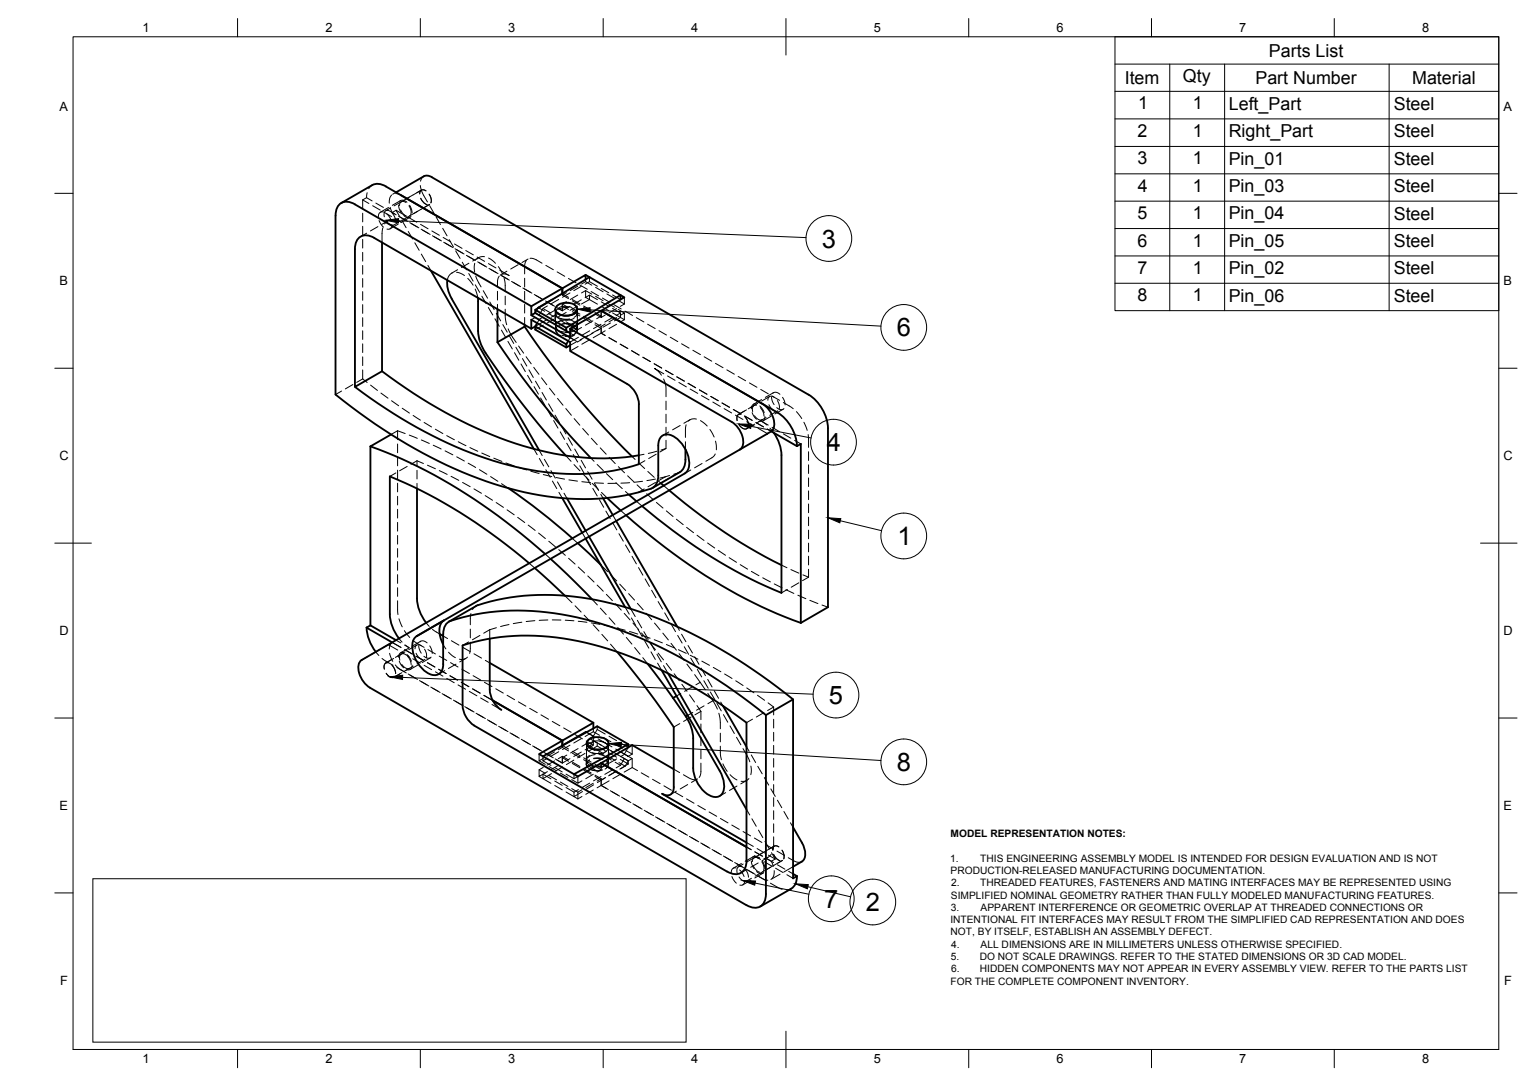
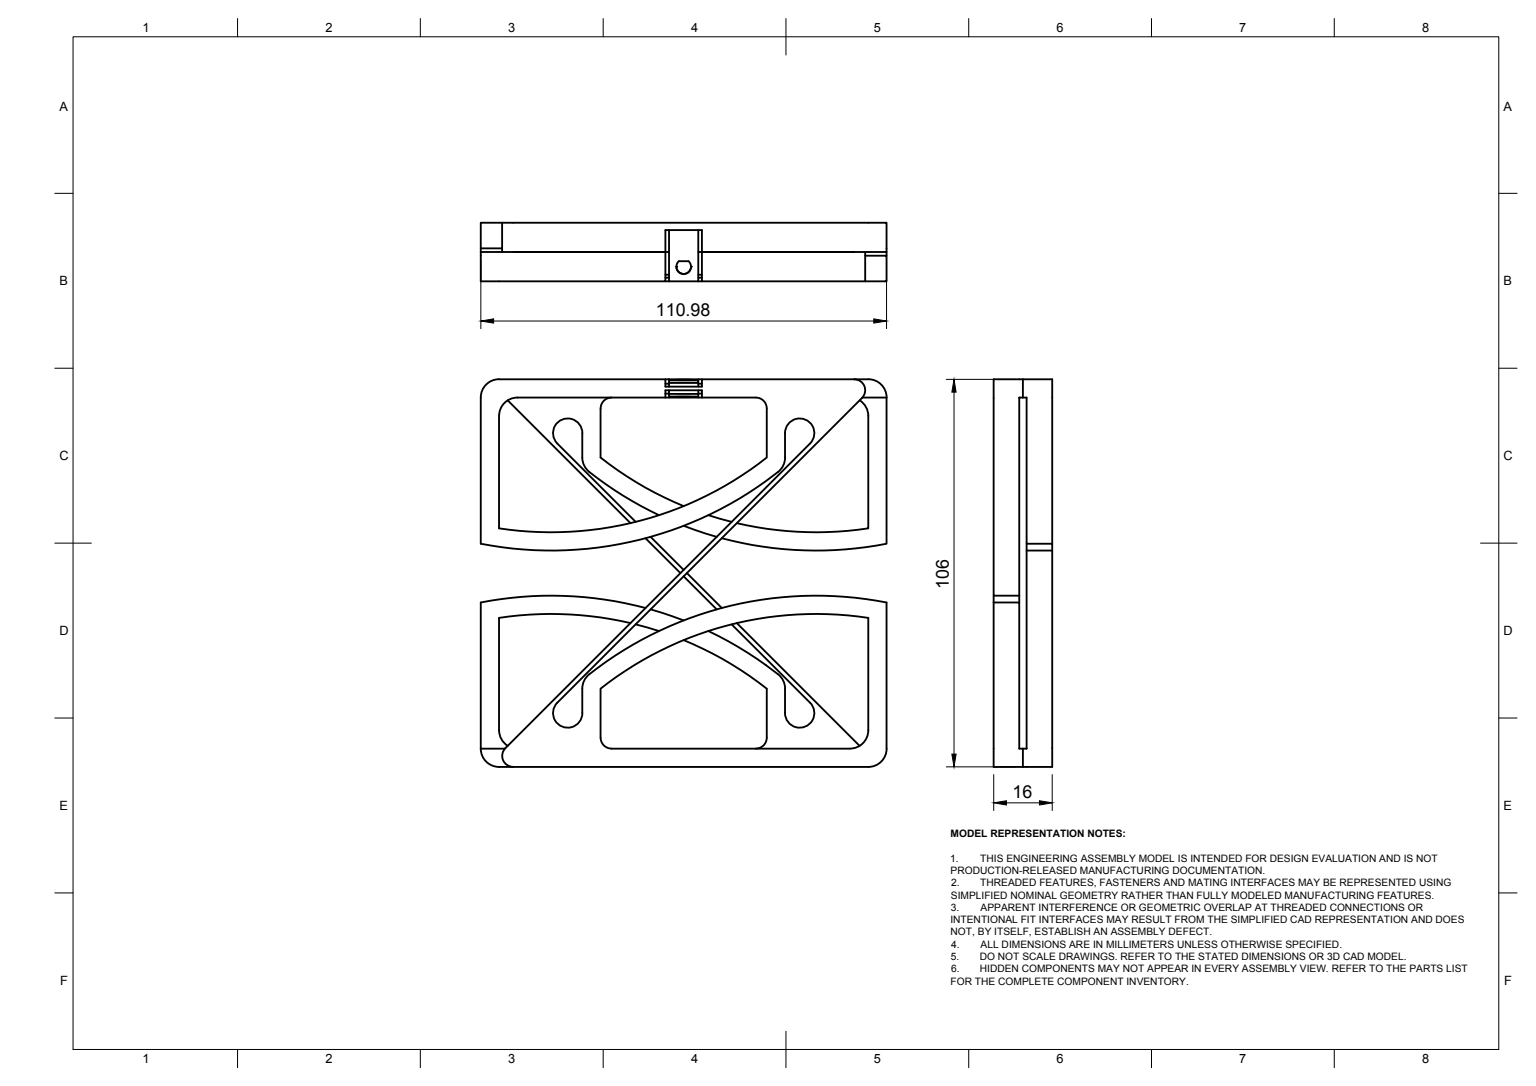
ISO-10303-21;
HEADER;
/* Generated by software containing ST-Developer
 * from STEP Tools, Inc. (www.steptools.com) 
 */

FILE_DESCRIPTION(
/* description */ (''),
/* implementation_level */ '2;1');

FILE_NAME(
/* name */ 'BR-159',
/* time_stamp */ '2026-10-05T13:12:53-07:00',
/* author */ (''),
/* organization */ (''),
/* preprocessor_version */ 'ST-DEVELOPER v20.2',
/* originating_system */ 'Autodesk Translation Framework v15.15.0.0',
/* authorisation */ '');

FILE_SCHEMA (('AUTOMOTIVE_DESIGN { 1 0 10303 214 3 1 1 }'));
ENDSEC;

DATA;
#10=MECHANICAL_DESIGN_GEOMETRIC_PRESENTATION_REPRESENTATION('',(#59,#60,
#61,#62,#63,#64,#65,#66),#5912);
#11=ITEM_DEFINED_TRANSFORMATION($,$,#3568,#3878);
#12=ITEM_DEFINED_TRANSFORMATION($,$,#3704,#3879);
#13=ITEM_DEFINED_TRANSFORMATION($,$,#3842,#3880);
#14=ITEM_DEFINED_TRANSFORMATION($,$,#3848,#3881);
#15=ITEM_DEFINED_TRANSFORMATION($,$,#3854,#3882);
#16=ITEM_DEFINED_TRANSFORMATION($,$,#3860,#3883);
#17=ITEM_DEFINED_TRANSFORMATION($,$,#3866,#3884);
#18=ITEM_DEFINED_TRANSFORMATION($,$,#3872,#3885);
#19=(
REPRESENTATION_RELATIONSHIP($,$,#5944,#5943)
REPRESENTATION_RELATIONSHIP_WITH_TRANSFORMATION(#11)
SHAPE_REPRESENTATION_RELATIONSHIP()
);
#20=(
REPRESENTATION_RELATIONSHIP($,$,#5945,#5943)
REPRESENTATION_RELATIONSHIP_WITH_TRANSFORMATION(#12)
SHAPE_REPRESENTATION_RELATIONSHIP()
);
#21=(
REPRESENTATION_RELATIONSHIP($,$,#5946,#5943)
REPRESENTATION_RELATIONSHIP_WITH_TRANSFORMATION(#13)
SHAPE_REPRESENTATION_RELATIONSHIP()
);
#22=(
REPRESENTATION_RELATIONSHIP($,$,#5947,#5943)
REPRESENTATION_RELATIONSHIP_WITH_TRANSFORMATION(#14)
SHAPE_REPRESENTATION_RELATIONSHIP()
);
#23=(
REPRESENTATION_RELATIONSHIP($,$,#5948,#5943)
REPRESENTATION_RELATIONSHIP_WITH_TRANSFORMATION(#15)
SHAPE_REPRESENTATION_RELATIONSHIP()
);
#24=(
REPRESENTATION_RELATIONSHIP($,$,#5949,#5943)
REPRESENTATION_RELATIONSHIP_WITH_TRANSFORMATION(#16)
SHAPE_REPRESENTATION_RELATIONSHIP()
);
#25=(
REPRESENTATION_RELATIONSHIP($,$,#5950,#5943)
REPRESENTATION_RELATIONSHIP_WITH_TRANSFORMATION(#17)
SHAPE_REPRESENTATION_RELATIONSHIP()
);
#26=(
REPRESENTATION_RELATIONSHIP($,$,#5951,#5943)
REPRESENTATION_RELATIONSHIP_WITH_TRANSFORMATION(#18)
SHAPE_REPRESENTATION_RELATIONSHIP()
);
#27=CONTEXT_DEPENDENT_SHAPE_REPRESENTATION(#19,#5935);
#28=CONTEXT_DEPENDENT_SHAPE_REPRESENTATION(#20,#5936);
#29=CONTEXT_DEPENDENT_SHAPE_REPRESENTATION(#21,#5937);
#30=CONTEXT_DEPENDENT_SHAPE_REPRESENTATION(#22,#5938);
#31=CONTEXT_DEPENDENT_SHAPE_REPRESENTATION(#23,#5939);
#32=CONTEXT_DEPENDENT_SHAPE_REPRESENTATION(#24,#5940);
#33=CONTEXT_DEPENDENT_SHAPE_REPRESENTATION(#25,#5941);
#34=CONTEXT_DEPENDENT_SHAPE_REPRESENTATION(#26,#5942);
#35=NEXT_ASSEMBLY_USAGE_OCCURRENCE('Left_Part:1','Left_Part:1',
'Left_Part:1',#5953,#5954,'Left_Part:1');
#36=NEXT_ASSEMBLY_USAGE_OCCURRENCE('Right_Part:1','Right_Part:1',
'Right_Part:1',#5953,#5955,'Right_Part:1');
#37=NEXT_ASSEMBLY_USAGE_OCCURRENCE('Pin_01:1','Pin_01:1','Pin_01:1',#5953,
#5956,'Pin_01:1');
#38=NEXT_ASSEMBLY_USAGE_OCCURRENCE('Pin_03:1','Pin_03:1','Pin_03:1',#5953,
#5957,'Pin_03:1');
#39=NEXT_ASSEMBLY_USAGE_OCCURRENCE('Pin_04:1','Pin_04:1','Pin_04:1',#5953,
#5958,'Pin_04:1');
#40=NEXT_ASSEMBLY_USAGE_OCCURRENCE('Pin_05:1','Pin_05:1','Pin_05:1',#5953,
#5959,'Pin_05:1');
#41=NEXT_ASSEMBLY_USAGE_OCCURRENCE('Pin_02:1','Pin_02:1','Pin_02:1',#5953,
#5960,'Pin_02:1');
#42=NEXT_ASSEMBLY_USAGE_OCCURRENCE('Pin_06:1','Pin_06:1','Pin_06:1',#5953,
#5961,'Pin_06:1');
#43=SHAPE_REPRESENTATION_RELATIONSHIP('SRR','None',#5944,#51);
#44=SHAPE_REPRESENTATION_RELATIONSHIP('SRR','None',#5945,#52);
#45=SHAPE_REPRESENTATION_RELATIONSHIP('SRR','None',#5946,#53);
#46=SHAPE_REPRESENTATION_RELATIONSHIP('SRR','None',#5947,#54);
#47=SHAPE_REPRESENTATION_RELATIONSHIP('SRR','None',#5948,#55);
#48=SHAPE_REPRESENTATION_RELATIONSHIP('SRR','None',#5949,#56);
#49=SHAPE_REPRESENTATION_RELATIONSHIP('SRR','None',#5950,#57);
#50=SHAPE_REPRESENTATION_RELATIONSHIP('SRR','None',#5951,#58);
#51=ADVANCED_BREP_SHAPE_REPRESENTATION('',(#67),#5904);
#52=ADVANCED_BREP_SHAPE_REPRESENTATION('',(#68),#5905);
#53=ADVANCED_BREP_SHAPE_REPRESENTATION('',(#69),#5906);
#54=ADVANCED_BREP_SHAPE_REPRESENTATION('',(#70),#5907);
#55=ADVANCED_BREP_SHAPE_REPRESENTATION('',(#71),#5908);
#56=ADVANCED_BREP_SHAPE_REPRESENTATION('',(#72),#5909);
#57=ADVANCED_BREP_SHAPE_REPRESENTATION('',(#73),#5910);
#58=ADVANCED_BREP_SHAPE_REPRESENTATION('',(#74),#5911);
#59=STYLED_ITEM('',(#5993),#67);
#60=STYLED_ITEM('',(#5993),#68);
#61=STYLED_ITEM('',(#5994),#69);
#62=STYLED_ITEM('',(#5994),#70);
#63=STYLED_ITEM('',(#5994),#71);
#64=STYLED_ITEM('',(#5994),#72);
#65=STYLED_ITEM('',(#5994),#73);
#66=STYLED_ITEM('',(#5994),#74);
#67=MANIFOLD_SOLID_BREP('Body1',#3470);
#68=MANIFOLD_SOLID_BREP('Body1',#3471);
#69=MANIFOLD_SOLID_BREP('Body1',#3472);
#70=MANIFOLD_SOLID_BREP('Body1',#3473);
#71=MANIFOLD_SOLID_BREP('Body1',#3474);
#72=MANIFOLD_SOLID_BREP('Body1',#3475);
#73=MANIFOLD_SOLID_BREP('Body1',#3476);
#74=MANIFOLD_SOLID_BREP('Body1',#3477);
#75=FACE_BOUND('',#374,.T.);
#76=FACE_BOUND('',#375,.T.);
#77=FACE_BOUND('',#379,.T.);
#78=FACE_BOUND('',#419,.T.);
#79=FACE_BOUND('',#421,.T.);
#80=FACE_BOUND('',#427,.T.);
#81=FACE_BOUND('',#428,.T.);
#82=FACE_BOUND('',#432,.T.);
#83=FACE_BOUND('',#437,.T.);
#84=FACE_BOUND('',#441,.T.);
#85=FACE_BOUND('',#442,.T.);
#86=FACE_BOUND('',#473,.T.);
#87=FACE_BOUND('',#474,.T.);
#88=FACE_BOUND('',#485,.T.);
#89=FACE_BOUND('',#489,.T.);
#90=FACE_BOUND('',#510,.T.);
#91=FACE_BOUND('',#511,.T.);
#92=FACE_BOUND('',#513,.T.);
#93=FACE_BOUND('',#515,.T.);
#94=FACE_BOUND('',#516,.T.);
#95=FACE_BOUND('',#522,.T.);
#96=ELLIPSE('',#3572,2.00043399581457,2.);
#97=ELLIPSE('',#3573,2.00173692551084,2.);
#98=ELLIPSE('',#3574,2.00173692551084,2.);
#99=ELLIPSE('',#3577,2.00043399581457,2.);
#100=ELLIPSE('',#3579,2.00043399581457,2.);
#101=ELLIPSE('',#3580,2.77129645175522,2.);
#102=ELLIPSE('',#3581,2.00043399581457,2.);
#103=ELLIPSE('',#3582,2.00043399581457,2.);
#104=ELLIPSE('',#3708,2.00043399581457,2.);
#105=ELLIPSE('',#3709,2.88922534092348,2.);
#106=ELLIPSE('',#3710,2.00043399581457,2.);
#107=ELLIPSE('',#3711,2.00173692551084,2.);
#108=ELLIPSE('',#3712,2.00173692551084,2.);
#109=ELLIPSE('',#3715,2.00043399581457,2.);
#110=ELLIPSE('',#3716,2.77129645175522,2.);
#111=ELLIPSE('',#3717,2.00043399581457,2.);
#112=ELLIPSE('',#3721,2.00043399581457,2.);
#113=ELLIPSE('',#3722,2.00043399581457,2.);
#114=CYLINDRICAL_SURFACE('',#3571,2.);
#115=CYLINDRICAL_SURFACE('',#3575,2.);
#116=CYLINDRICAL_SURFACE('',#3578,2.);
#117=CYLINDRICAL_SURFACE('',#3584,1.50000013517123);
#118=CYLINDRICAL_SURFACE('',#3588,1.4999996247669);
#119=CYLINDRICAL_SURFACE('',#3597,1.74999969554324);
#120=CYLINDRICAL_SURFACE('',#3601,4.99999999999999);
#121=CYLINDRICAL_SURFACE('',#3604,5.);
#122=CYLINDRICAL_SURFACE('',#3614,100.231846914414);
#123=CYLINDRICAL_SURFACE('',#3621,3.00000000000007);
#124=CYLINDRICAL_SURFACE('',#3625,95.2318469144141);
#125=CYLINDRICAL_SURFACE('',#3629,5.00000220964233);
#126=CYLINDRICAL_SURFACE('',#3633,3.99998589024062);
#127=CYLINDRICAL_SURFACE('',#3637,2.99999999999999);
#128=CYLINDRICAL_SURFACE('',#3640,3.00000000000001);
#129=CYLINDRICAL_SURFACE('',#3645,3.99998589024062);
#130=CYLINDRICAL_SURFACE('',#3649,5.00000220964233);
#131=CYLINDRICAL_SURFACE('',#3653,3.00000000000008);
#132=CYLINDRICAL_SURFACE('',#3656,2.99999999999999);
#133=CYLINDRICAL_SURFACE('',#3663,100.231846914414);
#134=CYLINDRICAL_SURFACE('',#3667,5.);
#135=CYLINDRICAL_SURFACE('',#3671,5.);
#136=CYLINDRICAL_SURFACE('',#3677,1.75000228959638);
#137=CYLINDRICAL_SURFACE('',#3694,95.231846914414);
#138=CYLINDRICAL_SURFACE('',#3707,2.);
#139=CYLINDRICAL_SURFACE('',#3713,2.);
#140=CYLINDRICAL_SURFACE('',#3720,2.);
#141=CYLINDRICAL_SURFACE('',#3723,1.50000013517123);
#142=CYLINDRICAL_SURFACE('',#3727,1.4999996247669);
#143=CYLINDRICAL_SURFACE('',#3732,5.);
#144=CYLINDRICAL_SURFACE('',#3735,5.);
#145=CYLINDRICAL_SURFACE('',#3739,1.75000228959638);
#146=CYLINDRICAL_SURFACE('',#3747,3.00000000000001);
#147=CYLINDRICAL_SURFACE('',#3751,3.99998589024062);
#148=CYLINDRICAL_SURFACE('',#3755,5.00000220964233);
#149=CYLINDRICAL_SURFACE('',#3758,95.231846914414);
#150=CYLINDRICAL_SURFACE('',#3762,3.00000000000008);
#151=CYLINDRICAL_SURFACE('',#3766,2.99999999999999);
#152=CYLINDRICAL_SURFACE('',#3779,100.231846914414);
#153=CYLINDRICAL_SURFACE('',#3794,1.74999969554324);
#154=CYLINDRICAL_SURFACE('',#3798,4.99999999999999);
#155=CYLINDRICAL_SURFACE('',#3801,5.);
#156=CYLINDRICAL_SURFACE('',#3820,100.231846914414);
#157=CYLINDRICAL_SURFACE('',#3832,3.00000000000007);
#158=CYLINDRICAL_SURFACE('',#3834,95.2318469144141);
#159=CYLINDRICAL_SURFACE('',#3836,5.00000220964233);
#160=CYLINDRICAL_SURFACE('',#3838,3.99998589024062);
#161=CYLINDRICAL_SURFACE('',#3840,2.99999999999999);
#162=CYLINDRICAL_SURFACE('',#3845,1.50000013517123);
#163=CYLINDRICAL_SURFACE('',#3849,1.4999996247669);
#164=CYLINDRICAL_SURFACE('',#3855,1.50000013517123);
#165=CYLINDRICAL_SURFACE('',#3861,2.);
#166=CYLINDRICAL_SURFACE('',#3869,1.4999996247669);
#167=CYLINDRICAL_SURFACE('',#3873,2.);
#168=FACE_OUTER_BOUND('',#350,.T.);
#169=FACE_OUTER_BOUND('',#351,.T.);
#170=FACE_OUTER_BOUND('',#352,.T.);
#171=FACE_OUTER_BOUND('',#353,.T.);
#172=FACE_OUTER_BOUND('',#354,.T.);
#173=FACE_OUTER_BOUND('',#355,.T.);
#174=FACE_OUTER_BOUND('',#356,.T.);
#175=FACE_OUTER_BOUND('',#357,.T.);
#176=FACE_OUTER_BOUND('',#358,.T.);
#177=FACE_OUTER_BOUND('',#359,.T.);
#178=FACE_OUTER_BOUND('',#360,.T.);
#179=FACE_OUTER_BOUND('',#361,.T.);
#180=FACE_OUTER_BOUND('',#362,.T.);
#181=FACE_OUTER_BOUND('',#363,.T.);
#182=FACE_OUTER_BOUND('',#364,.T.);
#183=FACE_OUTER_BOUND('',#365,.T.);
#184=FACE_OUTER_BOUND('',#366,.T.);
#185=FACE_OUTER_BOUND('',#367,.T.);
#186=FACE_OUTER_BOUND('',#368,.T.);
#187=FACE_OUTER_BOUND('',#369,.T.);
#188=FACE_OUTER_BOUND('',#370,.T.);
#189=FACE_OUTER_BOUND('',#371,.T.);
#190=FACE_OUTER_BOUND('',#372,.T.);
#191=FACE_OUTER_BOUND('',#373,.T.);
#192=FACE_OUTER_BOUND('',#376,.T.);
#193=FACE_OUTER_BOUND('',#377,.T.);
#194=FACE_OUTER_BOUND('',#378,.T.);
#195=FACE_OUTER_BOUND('',#380,.T.);
#196=FACE_OUTER_BOUND('',#381,.T.);
#197=FACE_OUTER_BOUND('',#382,.T.);
#198=FACE_OUTER_BOUND('',#383,.T.);
#199=FACE_OUTER_BOUND('',#384,.T.);
#200=FACE_OUTER_BOUND('',#385,.T.);
#201=FACE_OUTER_BOUND('',#386,.T.);
#202=FACE_OUTER_BOUND('',#387,.T.);
#203=FACE_OUTER_BOUND('',#388,.T.);
#204=FACE_OUTER_BOUND('',#389,.T.);
#205=FACE_OUTER_BOUND('',#390,.T.);
#206=FACE_OUTER_BOUND('',#391,.T.);
#207=FACE_OUTER_BOUND('',#392,.T.);
#208=FACE_OUTER_BOUND('',#393,.T.);
#209=FACE_OUTER_BOUND('',#394,.T.);
#210=FACE_OUTER_BOUND('',#395,.T.);
#211=FACE_OUTER_BOUND('',#396,.T.);
#212=FACE_OUTER_BOUND('',#397,.T.);
#213=FACE_OUTER_BOUND('',#398,.T.);
#214=FACE_OUTER_BOUND('',#399,.T.);
#215=FACE_OUTER_BOUND('',#400,.T.);
#216=FACE_OUTER_BOUND('',#401,.T.);
#217=FACE_OUTER_BOUND('',#402,.T.);
#218=FACE_OUTER_BOUND('',#403,.T.);
#219=FACE_OUTER_BOUND('',#404,.T.);
#220=FACE_OUTER_BOUND('',#405,.T.);
#221=FACE_OUTER_BOUND('',#406,.T.);
#222=FACE_OUTER_BOUND('',#407,.T.);
#223=FACE_OUTER_BOUND('',#408,.T.);
#224=FACE_OUTER_BOUND('',#409,.T.);
#225=FACE_OUTER_BOUND('',#410,.T.);
#226=FACE_OUTER_BOUND('',#411,.T.);
#227=FACE_OUTER_BOUND('',#412,.T.);
#228=FACE_OUTER_BOUND('',#413,.T.);
#229=FACE_OUTER_BOUND('',#414,.T.);
#230=FACE_OUTER_BOUND('',#415,.T.);
#231=FACE_OUTER_BOUND('',#416,.T.);
#232=FACE_OUTER_BOUND('',#417,.T.);
#233=FACE_OUTER_BOUND('',#418,.T.);
#234=FACE_OUTER_BOUND('',#420,.T.);
#235=FACE_OUTER_BOUND('',#422,.T.);
#236=FACE_OUTER_BOUND('',#423,.T.);
#237=FACE_OUTER_BOUND('',#424,.T.);
#238=FACE_OUTER_BOUND('',#425,.T.);
#239=FACE_OUTER_BOUND('',#426,.T.);
#240=FACE_OUTER_BOUND('',#429,.T.);
#241=FACE_OUTER_BOUND('',#430,.T.);
#242=FACE_OUTER_BOUND('',#431,.T.);
#243=FACE_OUTER_BOUND('',#433,.T.);
#244=FACE_OUTER_BOUND('',#434,.T.);
#245=FACE_OUTER_BOUND('',#435,.T.);
#246=FACE_OUTER_BOUND('',#436,.T.);
#247=FACE_OUTER_BOUND('',#438,.T.);
#248=FACE_OUTER_BOUND('',#439,.T.);
#249=FACE_OUTER_BOUND('',#440,.T.);
#250=FACE_OUTER_BOUND('',#443,.T.);
#251=FACE_OUTER_BOUND('',#444,.T.);
#252=FACE_OUTER_BOUND('',#445,.T.);
#253=FACE_OUTER_BOUND('',#446,.T.);
#254=FACE_OUTER_BOUND('',#447,.T.);
#255=FACE_OUTER_BOUND('',#448,.T.);
#256=FACE_OUTER_BOUND('',#449,.T.);
#257=FACE_OUTER_BOUND('',#450,.T.);
#258=FACE_OUTER_BOUND('',#451,.T.);
#259=FACE_OUTER_BOUND('',#452,.T.);
#260=FACE_OUTER_BOUND('',#453,.T.);
#261=FACE_OUTER_BOUND('',#454,.T.);
#262=FACE_OUTER_BOUND('',#455,.T.);
#263=FACE_OUTER_BOUND('',#456,.T.);
#264=FACE_OUTER_BOUND('',#457,.T.);
#265=FACE_OUTER_BOUND('',#458,.T.);
#266=FACE_OUTER_BOUND('',#459,.T.);
#267=FACE_OUTER_BOUND('',#460,.T.);
#268=FACE_OUTER_BOUND('',#461,.T.);
#269=FACE_OUTER_BOUND('',#462,.T.);
#270=FACE_OUTER_BOUND('',#463,.T.);
#271=FACE_OUTER_BOUND('',#464,.T.);
#272=FACE_OUTER_BOUND('',#465,.T.);
#273=FACE_OUTER_BOUND('',#466,.T.);
#274=FACE_OUTER_BOUND('',#467,.T.);
#275=FACE_OUTER_BOUND('',#468,.T.);
#276=FACE_OUTER_BOUND('',#469,.T.);
#277=FACE_OUTER_BOUND('',#470,.T.);
#278=FACE_OUTER_BOUND('',#471,.T.);
#279=FACE_OUTER_BOUND('',#472,.T.);
#280=FACE_OUTER_BOUND('',#475,.T.);
#281=FACE_OUTER_BOUND('',#476,.T.);
#282=FACE_OUTER_BOUND('',#477,.T.);
#283=FACE_OUTER_BOUND('',#478,.T.);
#284=FACE_OUTER_BOUND('',#479,.T.);
#285=FACE_OUTER_BOUND('',#480,.T.);
#286=FACE_OUTER_BOUND('',#481,.T.);
#287=FACE_OUTER_BOUND('',#482,.T.);
#288=FACE_OUTER_BOUND('',#483,.T.);
#289=FACE_OUTER_BOUND('',#484,.T.);
#290=FACE_OUTER_BOUND('',#486,.T.);
#291=FACE_OUTER_BOUND('',#487,.T.);
#292=FACE_OUTER_BOUND('',#488,.T.);
#293=FACE_OUTER_BOUND('',#490,.T.);
#294=FACE_OUTER_BOUND('',#491,.T.);
#295=FACE_OUTER_BOUND('',#492,.T.);
#296=FACE_OUTER_BOUND('',#493,.T.);
#297=FACE_OUTER_BOUND('',#494,.T.);
#298=FACE_OUTER_BOUND('',#495,.T.);
#299=FACE_OUTER_BOUND('',#496,.T.);
#300=FACE_OUTER_BOUND('',#497,.T.);
#301=FACE_OUTER_BOUND('',#498,.T.);
#302=FACE_OUTER_BOUND('',#499,.T.);
#303=FACE_OUTER_BOUND('',#500,.T.);
#304=FACE_OUTER_BOUND('',#501,.T.);
#305=FACE_OUTER_BOUND('',#502,.T.);
#306=FACE_OUTER_BOUND('',#503,.T.);
#307=FACE_OUTER_BOUND('',#504,.T.);
#308=FACE_OUTER_BOUND('',#505,.T.);
#309=FACE_OUTER_BOUND('',#506,.T.);
#310=FACE_OUTER_BOUND('',#507,.T.);
#311=FACE_OUTER_BOUND('',#508,.T.);
#312=FACE_OUTER_BOUND('',#509,.T.);
#313=FACE_OUTER_BOUND('',#512,.T.);
#314=FACE_OUTER_BOUND('',#514,.T.);
#315=FACE_OUTER_BOUND('',#517,.T.);
#316=FACE_OUTER_BOUND('',#518,.T.);
#317=FACE_OUTER_BOUND('',#519,.T.);
#318=FACE_OUTER_BOUND('',#520,.T.);
#319=FACE_OUTER_BOUND('',#521,.T.);
#320=FACE_OUTER_BOUND('',#523,.T.);
#321=FACE_OUTER_BOUND('',#524,.T.);
#322=FACE_OUTER_BOUND('',#525,.T.);
#323=FACE_OUTER_BOUND('',#526,.T.);
#324=FACE_OUTER_BOUND('',#527,.T.);
#325=FACE_OUTER_BOUND('',#528,.T.);
#326=FACE_OUTER_BOUND('',#529,.T.);
#327=FACE_OUTER_BOUND('',#530,.T.);
#328=FACE_OUTER_BOUND('',#531,.T.);
#329=FACE_OUTER_BOUND('',#532,.T.);
#330=FACE_OUTER_BOUND('',#533,.T.);
#331=FACE_OUTER_BOUND('',#534,.T.);
#332=FACE_OUTER_BOUND('',#535,.T.);
#333=FACE_OUTER_BOUND('',#536,.T.);
#334=FACE_OUTER_BOUND('',#537,.T.);
#335=FACE_OUTER_BOUND('',#538,.T.);
#336=FACE_OUTER_BOUND('',#539,.T.);
#337=FACE_OUTER_BOUND('',#540,.T.);
#338=FACE_OUTER_BOUND('',#541,.T.);
#339=FACE_OUTER_BOUND('',#542,.T.);
#340=FACE_OUTER_BOUND('',#543,.T.);
#341=FACE_OUTER_BOUND('',#544,.T.);
#342=FACE_OUTER_BOUND('',#545,.T.);
#343=FACE_OUTER_BOUND('',#546,.T.);
#344=FACE_OUTER_BOUND('',#547,.T.);
#345=FACE_OUTER_BOUND('',#548,.T.);
#346=FACE_OUTER_BOUND('',#549,.T.);
#347=FACE_OUTER_BOUND('',#550,.T.);
#348=FACE_OUTER_BOUND('',#551,.T.);
#349=FACE_OUTER_BOUND('',#552,.T.);
#350=EDGE_LOOP('',(#2190,#2191));
#351=EDGE_LOOP('',(#2192,#2193,#2194,#2195,#2196,#2197));
#352=EDGE_LOOP('',(#2198,#2199,#2200,#2201));
#353=EDGE_LOOP('',(#2202,#2203,#2204,#2205,#2206,#2207));
#354=EDGE_LOOP('',(#2208,#2209,#2210,#2211,#2212,#2213,#2214));
#355=EDGE_LOOP('',(#2215,#2216,#2217,#2218));
#356=EDGE_LOOP('',(#2219));
#357=EDGE_LOOP('',(#2220,#2221,#2222,#2223));
#358=EDGE_LOOP('',(#2224));
#359=EDGE_LOOP('',(#2225,#2226,#2227,#2228,#2229,#2230));
#360=EDGE_LOOP('',(#2231,#2232,#2233,#2234,#2235,#2236));
#361=EDGE_LOOP('',(#2237,#2238,#2239,#2240,#2241));
#362=EDGE_LOOP('',(#2242));
#363=EDGE_LOOP('',(#2243,#2244,#2245,#2246));
#364=EDGE_LOOP('',(#2247,#2248,#2249,#2250,#2251,#2252));
#365=EDGE_LOOP('',(#2253,#2254,#2255,#2256));
#366=EDGE_LOOP('',(#2257,#2258,#2259,#2260));
#367=EDGE_LOOP('',(#2261,#2262,#2263,#2264,#2265,#2266));
#368=EDGE_LOOP('',(#2267,#2268,#2269,#2270));
#369=EDGE_LOOP('',(#2271,#2272,#2273,#2274));
#370=EDGE_LOOP('',(#2275,#2276,#2277,#2278));
#371=EDGE_LOOP('',(#2279,#2280,#2281,#2282,#2283,#2284));
#372=EDGE_LOOP('',(#2285,#2286,#2287,#2288));
#373=EDGE_LOOP('',(#2289,#2290,#2291,#2292,#2293,#2294,#2295,#2296,#2297,
#2298,#2299,#2300));
#374=EDGE_LOOP('',(#2301));
#375=EDGE_LOOP('',(#2302));
#376=EDGE_LOOP('',(#2303,#2304,#2305,#2306));
#377=EDGE_LOOP('',(#2307,#2308,#2309,#2310,#2311,#2312));
#378=EDGE_LOOP('',(#2313,#2314,#2315,#2316));
#379=EDGE_LOOP('',(#2317));
#380=EDGE_LOOP('',(#2318,#2319,#2320,#2321,#2322,#2323));
#381=EDGE_LOOP('',(#2324,#2325,#2326,#2327,#2328,#2329));
#382=EDGE_LOOP('',(#2330,#2331,#2332,#2333));
#383=EDGE_LOOP('',(#2334,#2335,#2336,#2337));
#384=EDGE_LOOP('',(#2338,#2339,#2340,#2341));
#385=EDGE_LOOP('',(#2342,#2343,#2344,#2345));
#386=EDGE_LOOP('',(#2346,#2347,#2348,#2349));
#387=EDGE_LOOP('',(#2350,#2351,#2352,#2353));
#388=EDGE_LOOP('',(#2354,#2355,#2356,#2357));
#389=EDGE_LOOP('',(#2358,#2359,#2360,#2361,#2362));
#390=EDGE_LOOP('',(#2363,#2364,#2365,#2366,#2367,#2368,#2369));
#391=EDGE_LOOP('',(#2370,#2371,#2372,#2373,#2374));
#392=EDGE_LOOP('',(#2375,#2376,#2377,#2378));
#393=EDGE_LOOP('',(#2379,#2380,#2381,#2382));
#394=EDGE_LOOP('',(#2383,#2384,#2385,#2386));
#395=EDGE_LOOP('',(#2387,#2388,#2389,#2390));
#396=EDGE_LOOP('',(#2391,#2392,#2393,#2394));
#397=EDGE_LOOP('',(#2395,#2396,#2397,#2398));
#398=EDGE_LOOP('',(#2399,#2400,#2401,#2402));
#399=EDGE_LOOP('',(#2403,#2404,#2405,#2406));
#400=EDGE_LOOP('',(#2407,#2408,#2409,#2410));
#401=EDGE_LOOP('',(#2411,#2412,#2413,#2414,#2415,#2416));
#402=EDGE_LOOP('',(#2417,#2418,#2419,#2420,#2421,#2422));
#403=EDGE_LOOP('',(#2423,#2424,#2425,#2426));
#404=EDGE_LOOP('',(#2427,#2428,#2429,#2430));
#405=EDGE_LOOP('',(#2431,#2432,#2433,#2434));
#406=EDGE_LOOP('',(#2435,#2436,#2437,#2438,#2439));
#407=EDGE_LOOP('',(#2440,#2441,#2442,#2443,#2444,#2445,#2446,#2447,#2448,
#2449,#2450));
#408=EDGE_LOOP('',(#2451,#2452,#2453,#2454));
#409=EDGE_LOOP('',(#2455,#2456,#2457,#2458));
#410=EDGE_LOOP('',(#2459,#2460,#2461,#2462,#2463,#2464,#2465,#2466,#2467,
#2468,#2469,#2470,#2471,#2472,#2473,#2474,#2475,#2476,#2477,#2478,#2479,
#2480,#2481,#2482,#2483,#2484,#2485,#2486,#2487));
#411=EDGE_LOOP('',(#2488,#2489,#2490,#2491));
#412=EDGE_LOOP('',(#2492));
#413=EDGE_LOOP('',(#2493,#2494,#2495,#2496));
#414=EDGE_LOOP('',(#2497,#2498,#2499,#2500,#2501,#2502,#2503,#2504));
#415=EDGE_LOOP('',(#2505,#2506,#2507,#2508));
#416=EDGE_LOOP('',(#2509,#2510,#2511,#2512));
#417=EDGE_LOOP('',(#2513,#2514,#2515,#2516));
#418=EDGE_LOOP('',(#2517,#2518,#2519,#2520));
#419=EDGE_LOOP('',(#2521));
#420=EDGE_LOOP('',(#2522,#2523,#2524,#2525));
#421=EDGE_LOOP('',(#2526));
#422=EDGE_LOOP('',(#2527,#2528,#2529,#2530));
#423=EDGE_LOOP('',(#2531,#2532,#2533,#2534));
#424=EDGE_LOOP('',(#2535,#2536,#2537,#2538,#2539,#2540));
#425=EDGE_LOOP('',(#2541,#2542,#2543,#2544,#2545,#2546));
#426=EDGE_LOOP('',(#2547,#2548,#2549,#2550,#2551,#2552,#2553,#2554,#2555,
#2556,#2557,#2558,#2559,#2560,#2561,#2562,#2563,#2564,#2565,#2566,#2567,
#2568,#2569));
#427=EDGE_LOOP('',(#2570,#2571,#2572,#2573,#2574,#2575,#2576,#2577,#2578,
#2579));
#428=EDGE_LOOP('',(#2580,#2581,#2582,#2583,#2584,#2585));
#429=EDGE_LOOP('',(#2586,#2587,#2588,#2589));
#430=EDGE_LOOP('',(#2590,#2591,#2592,#2593,#2594,#2595,#2596,#2597,#2598,
#2599,#2600,#2601,#2602,#2603));
#431=EDGE_LOOP('',(#2604,#2605,#2606,#2607));
#432=EDGE_LOOP('',(#2608,#2609,#2610));
#433=EDGE_LOOP('',(#2611,#2612,#2613,#2614));
#434=EDGE_LOOP('',(#2615,#2616,#2617,#2618));
#435=EDGE_LOOP('',(#2619,#2620,#2621,#2622));
#436=EDGE_LOOP('',(#2623,#2624,#2625,#2626));
#437=EDGE_LOOP('',(#2627));
#438=EDGE_LOOP('',(#2628,#2629,#2630,#2631,#2632,#2633,#2634,#2635));
#439=EDGE_LOOP('',(#2636,#2637,#2638,#2639));
#440=EDGE_LOOP('',(#2640,#2641,#2642,#2643,#2644,#2645,#2646,#2647,#2648,
#2649,#2650,#2651));
#441=EDGE_LOOP('',(#2652));
#442=EDGE_LOOP('',(#2653));
#443=EDGE_LOOP('',(#2654,#2655));
#444=EDGE_LOOP('',(#2656,#2657,#2658,#2659,#2660,#2661,#2662,#2663));
#445=EDGE_LOOP('',(#2664,#2665,#2666,#2667,#2668,#2669));
#446=EDGE_LOOP('',(#2670,#2671,#2672,#2673,#2674,#2675,#2676));
#447=EDGE_LOOP('',(#2677,#2678,#2679,#2680,#2681,#2682,#2683));
#448=EDGE_LOOP('',(#2684,#2685,#2686,#2687));
#449=EDGE_LOOP('',(#2688,#2689,#2690,#2691));
#450=EDGE_LOOP('',(#2692));
#451=EDGE_LOOP('',(#2693,#2694,#2695,#2696));
#452=EDGE_LOOP('',(#2697));
#453=EDGE_LOOP('',(#2698,#2699,#2700,#2701));
#454=EDGE_LOOP('',(#2702,#2703,#2704,#2705,#2706));
#455=EDGE_LOOP('',(#2707,#2708,#2709,#2710));
#456=EDGE_LOOP('',(#2711,#2712,#2713,#2714));
#457=EDGE_LOOP('',(#2715,#2716,#2717,#2718));
#458=EDGE_LOOP('',(#2719));
#459=EDGE_LOOP('',(#2720,#2721,#2722,#2723));
#460=EDGE_LOOP('',(#2724,#2725,#2726,#2727));
#461=EDGE_LOOP('',(#2728,#2729,#2730,#2731,#2732,#2733));
#462=EDGE_LOOP('',(#2734,#2735,#2736,#2737,#2738,#2739));
#463=EDGE_LOOP('',(#2740,#2741,#2742,#2743,#2744));
#464=EDGE_LOOP('',(#2745,#2746,#2747,#2748));
#465=EDGE_LOOP('',(#2749,#2750,#2751,#2752));
#466=EDGE_LOOP('',(#2753,#2754,#2755,#2756));
#467=EDGE_LOOP('',(#2757,#2758,#2759,#2760));
#468=EDGE_LOOP('',(#2761,#2762,#2763,#2764));
#469=EDGE_LOOP('',(#2765,#2766,#2767,#2768));
#470=EDGE_LOOP('',(#2769,#2770,#2771,#2772,#2773,#2774,#2775,#2776,#2777,
#2778,#2779,#2780,#2781,#2782));
#471=EDGE_LOOP('',(#2783,#2784,#2785,#2786));
#472=EDGE_LOOP('',(#2787,#2788,#2789,#2790,#2791,#2792,#2793,#2794,#2795,
#2796,#2797,#2798));
#473=EDGE_LOOP('',(#2799));
#474=EDGE_LOOP('',(#2800));
#475=EDGE_LOOP('',(#2801,#2802,#2803,#2804));
#476=EDGE_LOOP('',(#2805,#2806,#2807,#2808));
#477=EDGE_LOOP('',(#2809,#2810,#2811,#2812));
#478=EDGE_LOOP('',(#2813,#2814,#2815,#2816,#2817,#2818));
#479=EDGE_LOOP('',(#2819,#2820,#2821,#2822,#2823,#2824,#2825,#2826));
#480=EDGE_LOOP('',(#2827,#2828,#2829,#2830,#2831,#2832));
#481=EDGE_LOOP('',(#2833,#2834,#2835,#2836));
#482=EDGE_LOOP('',(#2837,#2838,#2839,#2840));
#483=EDGE_LOOP('',(#2841,#2842,#2843,#2844,#2845,#2846));
#484=EDGE_LOOP('',(#2847,#2848,#2849,#2850));
#485=EDGE_LOOP('',(#2851));
#486=EDGE_LOOP('',(#2852,#2853,#2854,#2855));
#487=EDGE_LOOP('',(#2856,#2857,#2858,#2859,#2860,#2861,#2862,#2863,#2864,
#2865,#2866));
#488=EDGE_LOOP('',(#2867,#2868,#2869,#2870));
#489=EDGE_LOOP('',(#2871,#2872,#2873));
#490=EDGE_LOOP('',(#2874,#2875,#2876,#2877));
#491=EDGE_LOOP('',(#2878,#2879,#2880,#2881));
#492=EDGE_LOOP('',(#2882,#2883,#2884,#2885,#2886,#2887));
#493=EDGE_LOOP('',(#2888,#2889,#2890,#2891,#2892,#2893,#2894,#2895));
#494=EDGE_LOOP('',(#2896,#2897,#2898,#2899));
#495=EDGE_LOOP('',(#2900,#2901,#2902,#2903,#2904,#2905));
#496=EDGE_LOOP('',(#2906,#2907,#2908,#2909,#2910,#2911));
#497=EDGE_LOOP('',(#2912,#2913,#2914,#2915,#2916));
#498=EDGE_LOOP('',(#2917));
#499=EDGE_LOOP('',(#2918,#2919,#2920,#2921));
#500=EDGE_LOOP('',(#2922,#2923,#2924,#2925,#2926,#2927));
#501=EDGE_LOOP('',(#2928,#2929,#2930,#2931));
#502=EDGE_LOOP('',(#2932,#2933,#2934,#2935));
#503=EDGE_LOOP('',(#2936,#2937,#2938,#2939,#2940,#2941));
#504=EDGE_LOOP('',(#2942,#2943,#2944,#2945));
#505=EDGE_LOOP('',(#2946,#2947,#2948,#2949));
#506=EDGE_LOOP('',(#2950,#2951,#2952,#2953));
#507=EDGE_LOOP('',(#2954,#2955,#2956,#2957));
#508=EDGE_LOOP('',(#2958,#2959,#2960,#2961));
#509=EDGE_LOOP('',(#2962,#2963,#2964,#2965,#2966,#2967,#2968,#2969,#2970,
#2971,#2972,#2973,#2974,#2975,#2976,#2977,#2978,#2979,#2980,#2981,#2982,
#2983,#2984));
#510=EDGE_LOOP('',(#2985,#2986,#2987,#2988,#2989,#2990,#2991,#2992,#2993,
#2994));
#511=EDGE_LOOP('',(#2995,#2996,#2997,#2998,#2999,#3000));
#512=EDGE_LOOP('',(#3001,#3002,#3003,#3004));
#513=EDGE_LOOP('',(#3005));
#514=EDGE_LOOP('',(#3006,#3007,#3008,#3009,#3010,#3011,#3012,#3013,#3014,
#3015,#3016,#3017));
#515=EDGE_LOOP('',(#3018));
#516=EDGE_LOOP('',(#3019));
#517=EDGE_LOOP('',(#3020,#3021,#3022,#3023));
#518=EDGE_LOOP('',(#3024,#3025,#3026,#3027));
#519=EDGE_LOOP('',(#3028,#3029,#3030,#3031,#3032,#3033,#3034,#3035,#3036,
#3037,#3038,#3039,#3040,#3041,#3042,#3043,#3044,#3045,#3046,#3047,#3048,
#3049,#3050,#3051,#3052,#3053,#3054,#3055,#3056));
#520=EDGE_LOOP('',(#3057,#3058,#3059,#3060,#3061,#3062));
#521=EDGE_LOOP('',(#3063,#3064,#3065,#3066));
#522=EDGE_LOOP('',(#3067));
#523=EDGE_LOOP('',(#3068,#3069,#3070,#3071,#3072,#3073));
#524=EDGE_LOOP('',(#3074,#3075,#3076,#3077,#3078,#3079));
#525=EDGE_LOOP('',(#3080,#3081,#3082,#3083));
#526=EDGE_LOOP('',(#3084,#3085,#3086,#3087));
#527=EDGE_LOOP('',(#3088,#3089,#3090,#3091));
#528=EDGE_LOOP('',(#3092,#3093,#3094,#3095));
#529=EDGE_LOOP('',(#3096,#3097,#3098,#3099));
#530=EDGE_LOOP('',(#3100,#3101,#3102,#3103));
#531=EDGE_LOOP('',(#3104,#3105,#3106,#3107));
#532=EDGE_LOOP('',(#3108,#3109,#3110,#3111,#3112));
#533=EDGE_LOOP('',(#3113,#3114,#3115,#3116,#3117,#3118,#3119));
#534=EDGE_LOOP('',(#3120,#3121,#3122,#3123));
#535=EDGE_LOOP('',(#3124));
#536=EDGE_LOOP('',(#3125,#3126,#3127,#3128));
#537=EDGE_LOOP('',(#3129));
#538=EDGE_LOOP('',(#3130,#3131,#3132,#3133));
#539=EDGE_LOOP('',(#3134));
#540=EDGE_LOOP('',(#3135));
#541=EDGE_LOOP('',(#3136,#3137,#3138,#3139));
#542=EDGE_LOOP('',(#3140));
#543=EDGE_LOOP('',(#3141));
#544=EDGE_LOOP('',(#3142,#3143,#3144,#3145));
#545=EDGE_LOOP('',(#3146));
#546=EDGE_LOOP('',(#3147));
#547=EDGE_LOOP('',(#3148));
#548=EDGE_LOOP('',(#3149,#3150,#3151,#3152));
#549=EDGE_LOOP('',(#3153));
#550=EDGE_LOOP('',(#3154,#3155,#3156,#3157));
#551=EDGE_LOOP('',(#3158));
#552=EDGE_LOOP('',(#3159));
#553=CIRCLE('',#3570,2.);
#554=CIRCLE('',#3576,2.);
#555=CIRCLE('',#3585,1.50000013517123);
#556=CIRCLE('',#3586,1.50000013517123);
#557=CIRCLE('',#3589,1.4999996247669);
#558=CIRCLE('',#3590,1.4999996247669);
#559=CIRCLE('',#3596,1.74999969554324);
#560=CIRCLE('',#3598,1.74999969554324);
#561=CIRCLE('',#3602,4.99999999999999);
#562=CIRCLE('',#3603,4.99999999999999);
#563=CIRCLE('',#3605,5.);
#564=CIRCLE('',#3606,5.);
#565=CIRCLE('',#3613,2.99999999999999);
#566=CIRCLE('',#3615,100.231846914414);
#567=CIRCLE('',#3616,100.231846914414);
#568=CIRCLE('',#3622,3.00000000000007);
#569=CIRCLE('',#3623,3.00000000000007);
#570=CIRCLE('',#3626,95.2318469144141);
#571=CIRCLE('',#3627,95.2318469144141);
#572=CIRCLE('',#3630,5.00000220964233);
#573=CIRCLE('',#3631,5.00000220964233);
#574=CIRCLE('',#3634,3.99998589024062);
#575=CIRCLE('',#3635,3.99998589024062);
#576=CIRCLE('',#3638,2.99999999999999);
#577=CIRCLE('',#3639,2.99999999999999);
#578=CIRCLE('',#3641,3.00000000000001);
#579=CIRCLE('',#3642,3.00000000000001);
#580=CIRCLE('',#3643,3.00000000000001);
#581=CIRCLE('',#3646,3.99998589024062);
#582=CIRCLE('',#3647,3.99998589024062);
#583=CIRCLE('',#3650,5.00000220964233);
#584=CIRCLE('',#3651,5.00000220964233);
#585=CIRCLE('',#3654,3.00000000000008);
#586=CIRCLE('',#3655,3.00000000000008);
#587=CIRCLE('',#3657,2.99999999999999);
#588=CIRCLE('',#3664,100.231846914414);
#589=CIRCLE('',#3665,100.231846914414);
#590=CIRCLE('',#3668,5.);
#591=CIRCLE('',#3669,5.);
#592=CIRCLE('',#3672,5.);
#593=CIRCLE('',#3673,5.);
#594=CIRCLE('',#3676,95.231846914414);
#595=CIRCLE('',#3678,1.75000228959638);
#596=CIRCLE('',#3679,1.75000228959638);
#597=CIRCLE('',#3693,95.231846914414);
#598=CIRCLE('',#3706,2.);
#599=CIRCLE('',#3714,2.);
#600=CIRCLE('',#3724,1.50000013517123);
#601=CIRCLE('',#3725,1.50000013517123);
#602=CIRCLE('',#3728,1.4999996247669);
#603=CIRCLE('',#3729,1.4999996247669);
#604=CIRCLE('',#3733,5.);
#605=CIRCLE('',#3734,5.);
#606=CIRCLE('',#3736,5.);
#607=CIRCLE('',#3737,5.);
#608=CIRCLE('',#3740,1.75000228959638);
#609=CIRCLE('',#3741,1.75000228959638);
#610=CIRCLE('',#3748,3.00000000000001);
#611=CIRCLE('',#3749,3.00000000000001);
#612=CIRCLE('',#3750,3.00000000000001);
#613=CIRCLE('',#3752,3.99998589024062);
#614=CIRCLE('',#3753,3.99998589024062);
#615=CIRCLE('',#3756,5.00000220964233);
#616=CIRCLE('',#3757,5.00000220964233);
#617=CIRCLE('',#3759,95.231846914414);
#618=CIRCLE('',#3760,95.231846914414);
#619=CIRCLE('',#3763,3.00000000000008);
#620=CIRCLE('',#3764,3.00000000000008);
#621=CIRCLE('',#3767,2.99999999999999);
#622=CIRCLE('',#3780,100.231846914414);
#623=CIRCLE('',#3781,100.231846914414);
#624=CIRCLE('',#3793,1.74999969554324);
#625=CIRCLE('',#3795,1.74999969554324);
#626=CIRCLE('',#3799,4.99999999999999);
#627=CIRCLE('',#3800,4.99999999999999);
#628=CIRCLE('',#3802,5.);
#629=CIRCLE('',#3803,5.);
#630=CIRCLE('',#3810,2.99999999999999);
#631=CIRCLE('',#3811,100.231846914414);
#632=CIRCLE('',#3812,5.00000220964233);
#633=CIRCLE('',#3813,3.99998589024062);
#634=CIRCLE('',#3814,3.00000000000007);
#635=CIRCLE('',#3815,95.2318469144141);
#636=CIRCLE('',#3818,2.99999999999999);
#637=CIRCLE('',#3821,100.231846914414);
#638=CIRCLE('',#3823,3.99998589024062);
#639=CIRCLE('',#3824,5.00000220964233);
#640=CIRCLE('',#3825,95.2318469144141);
#641=CIRCLE('',#3826,3.00000000000007);
#642=CIRCLE('',#3827,2.99999999999999);
#643=CIRCLE('',#3844,1.50000013517123);
#644=CIRCLE('',#3846,1.50000013517123);
#645=CIRCLE('',#3850,1.4999996247669);
#646=CIRCLE('',#3851,1.4999996247669);
#647=CIRCLE('',#3856,1.50000013517123);
#648=CIRCLE('',#3857,1.50000013517123);
#649=CIRCLE('',#3862,2.);
#650=CIRCLE('',#3863,2.);
#651=CIRCLE('',#3868,1.4999996247669);
#652=CIRCLE('',#3870,1.4999996247669);
#653=CIRCLE('',#3874,2.);
#654=CIRCLE('',#3875,2.);
#655=LINE('',#4894,#1020);
#656=LINE('',#4900,#1021);
#657=LINE('',#4907,#1022);
#658=LINE('',#4917,#1023);
#659=LINE('',#4921,#1024);
#660=LINE('',#4923,#1025);
#661=LINE('',#4925,#1026);
#662=LINE('',#4927,#1027);
#663=LINE('',#4928,#1028);
#664=LINE('',#4933,#1029);
#665=LINE('',#4940,#1030);
#666=LINE('',#4945,#1031);
#667=LINE('',#4947,#1032);
#668=LINE('',#4949,#1033);
#669=LINE('',#4951,#1034);
#670=LINE('',#4952,#1035);
#671=LINE('',#4956,#1036);
#672=LINE('',#4958,#1037);
#673=LINE('',#4960,#1038);
#674=LINE('',#4962,#1039);
#675=LINE('',#4964,#1040);
#676=LINE('',#4965,#1041);
#677=LINE('',#4968,#1042);
#678=LINE('',#4970,#1043);
#679=LINE('',#4972,#1044);
#680=LINE('',#4973,#1045);
#681=LINE('',#4979,#1046);
#682=LINE('',#4983,#1047);
#683=LINE('',#4985,#1048);
#684=LINE('',#4987,#1049);
#685=LINE('',#4989,#1050);
#686=LINE('',#4990,#1051);
#687=LINE('',#4994,#1052);
#688=LINE('',#4996,#1053);
#689=LINE('',#4998,#1054);
#690=LINE('',#4999,#1055);
#691=LINE('',#5007,#1056);
#692=LINE('',#5010,#1057);
#693=LINE('',#5012,#1058);
#694=LINE('',#5013,#1059);
#695=LINE('',#5016,#1060);
#696=LINE('',#5018,#1061);
#697=LINE('',#5019,#1062);
#698=LINE('',#5022,#1063);
#699=LINE('',#5023,#1064);
#700=LINE('',#5026,#1065);
#701=LINE('',#5027,#1066);
#702=LINE('',#5030,#1067);
#703=LINE('',#5031,#1068);
#704=LINE('',#5034,#1069);
#705=LINE('',#5036,#1070);
#706=LINE('',#5038,#1071);
#707=LINE('',#5042,#1072);
#708=LINE('',#5043,#1073);
#709=LINE('',#5048,#1074);
#710=LINE('',#5052,#1075);
#711=LINE('',#5053,#1076);
#712=LINE('',#5055,#1077);
#713=LINE('',#5058,#1078);
#714=LINE('',#5059,#1079);
#715=LINE('',#5062,#1080);
#716=LINE('',#5064,#1081);
#717=LINE('',#5066,#1082);
#718=LINE('',#5067,#1083);
#719=LINE('',#5073,#1084);
#720=LINE('',#5076,#1085);
#721=LINE('',#5078,#1086);
#722=LINE('',#5079,#1087);
#723=LINE('',#5085,#1088);
#724=LINE('',#5087,#1089);
#725=LINE('',#5088,#1090);
#726=LINE('',#5094,#1091);
#727=LINE('',#5097,#1092);
#728=LINE('',#5099,#1093);
#729=LINE('',#5100,#1094);
#730=LINE('',#5106,#1095);
#731=LINE('',#5109,#1096);
#732=LINE('',#5111,#1097);
#733=LINE('',#5112,#1098);
#734=LINE('',#5117,#1099);
#735=LINE('',#5124,#1100);
#736=LINE('',#5129,#1101);
#737=LINE('',#5132,#1102);
#738=LINE('',#5134,#1103);
#739=LINE('',#5135,#1104);
#740=LINE('',#5140,#1105);
#741=LINE('',#5144,#1106);
#742=LINE('',#5146,#1107);
#743=LINE('',#5147,#1108);
#744=LINE('',#5152,#1109);
#745=LINE('',#5157,#1110);
#746=LINE('',#5159,#1111);
#747=LINE('',#5161,#1112);
#748=LINE('',#5162,#1113);
#749=LINE('',#5167,#1114);
#750=LINE('',#5171,#1115);
#751=LINE('',#5174,#1116);
#752=LINE('',#5178,#1117);
#753=LINE('',#5180,#1118);
#754=LINE('',#5182,#1119);
#755=LINE('',#5183,#1120);
#756=LINE('',#5187,#1121);
#757=LINE('',#5189,#1122);
#758=LINE('',#5191,#1123);
#759=LINE('',#5192,#1124);
#760=LINE('',#5196,#1125);
#761=LINE('',#5198,#1126);
#762=LINE('',#5200,#1127);
#763=LINE('',#5202,#1128);
#764=LINE('',#5204,#1129);
#765=LINE('',#5205,#1130);
#766=LINE('',#5209,#1131);
#767=LINE('',#5211,#1132);
#768=LINE('',#5213,#1133);
#769=LINE('',#5215,#1134);
#770=LINE('',#5217,#1135);
#771=LINE('',#5218,#1136);
#772=LINE('',#5220,#1137);
#773=LINE('',#5221,#1138);
#774=LINE('',#5226,#1139);
#775=LINE('',#5230,#1140);
#776=LINE('',#5232,#1141);
#777=LINE('',#5233,#1142);
#778=LINE('',#5238,#1143);
#779=LINE('',#5241,#1144);
#780=LINE('',#5244,#1145);
#781=LINE('',#5246,#1146);
#782=LINE('',#5248,#1147);
#783=LINE('',#5249,#1148);
#784=LINE('',#5250,#1149);
#785=LINE('',#5251,#1150);
#786=LINE('',#5252,#1151);
#787=LINE('',#5258,#1152);
#788=LINE('',#5261,#1153);
#789=LINE('',#5264,#1154);
#790=LINE('',#5266,#1155);
#791=LINE('',#5267,#1156);
#792=LINE('',#5269,#1157);
#793=LINE('',#5271,#1158);
#794=LINE('',#5276,#1159);
#795=LINE('',#5282,#1160);
#796=LINE('',#5284,#1161);
#797=LINE('',#5286,#1162);
#798=LINE('',#5287,#1163);
#799=LINE('',#5290,#1164);
#800=LINE('',#5291,#1165);
#801=LINE('',#5293,#1166);
#802=LINE('',#5294,#1167);
#803=LINE('',#5297,#1168);
#804=LINE('',#5298,#1169);
#805=LINE('',#5300,#1170);
#806=LINE('',#5303,#1171);
#807=LINE('',#5305,#1172);
#808=LINE('',#5306,#1173);
#809=LINE('',#5308,#1174);
#810=LINE('',#5311,#1175);
#811=LINE('',#5312,#1176);
#812=LINE('',#5315,#1177);
#813=LINE('',#5316,#1178);
#814=LINE('',#5318,#1179);
#815=LINE('',#5323,#1180);
#816=LINE('',#5325,#1181);
#817=LINE('',#5327,#1182);
#818=LINE('',#5329,#1183);
#819=LINE('',#5331,#1184);
#820=LINE('',#5332,#1185);
#821=LINE('',#5335,#1186);
#822=LINE('',#5338,#1187);
#823=LINE('',#5339,#1188);
#824=LINE('',#5340,#1189);
#825=LINE('',#5341,#1190);
#826=LINE('',#5342,#1191);
#827=LINE('',#5344,#1192);
#828=LINE('',#5346,#1193);
#829=LINE('',#5348,#1194);
#830=LINE('',#5350,#1195);
#831=LINE('',#5352,#1196);
#832=LINE('',#5354,#1197);
#833=LINE('',#5356,#1198);
#834=LINE('',#5362,#1199);
#835=LINE('',#5372,#1200);
#836=LINE('',#5379,#1201);
#837=LINE('',#5387,#1202);
#838=LINE('',#5389,#1203);
#839=LINE('',#5391,#1204);
#840=LINE('',#5393,#1205);
#841=LINE('',#5394,#1206);
#842=LINE('',#5397,#1207);
#843=LINE('',#5399,#1208);
#844=LINE('',#5401,#1209);
#845=LINE('',#5403,#1210);
#846=LINE('',#5404,#1211);
#847=LINE('',#5409,#1212);
#848=LINE('',#5415,#1213);
#849=LINE('',#5422,#1214);
#850=LINE('',#5428,#1215);
#851=LINE('',#5430,#1216);
#852=LINE('',#5432,#1217);
#853=LINE('',#5433,#1218);
#854=LINE('',#5438,#1219);
#855=LINE('',#5441,#1220);
#856=LINE('',#5447,#1221);
#857=LINE('',#5450,#1222);
#858=LINE('',#5453,#1223);
#859=LINE('',#5455,#1224);
#860=LINE('',#5456,#1225);
#861=LINE('',#5461,#1226);
#862=LINE('',#5467,#1227);
#863=LINE('',#5469,#1228);
#864=LINE('',#5471,#1229);
#865=LINE('',#5472,#1230);
#866=LINE('',#5476,#1231);
#867=LINE('',#5478,#1232);
#868=LINE('',#5480,#1233);
#869=LINE('',#5481,#1234);
#870=LINE('',#5485,#1235);
#871=LINE('',#5487,#1236);
#872=LINE('',#5488,#1237);
#873=LINE('',#5490,#1238);
#874=LINE('',#5491,#1239);
#875=LINE('',#5495,#1240);
#876=LINE('',#5497,#1241);
#877=LINE('',#5498,#1242);
#878=LINE('',#5500,#1243);
#879=LINE('',#5501,#1244);
#880=LINE('',#5507,#1245);
#881=LINE('',#5512,#1246);
#882=LINE('',#5518,#1247);
#883=LINE('',#5521,#1248);
#884=LINE('',#5524,#1249);
#885=LINE('',#5526,#1250);
#886=LINE('',#5527,#1251);
#887=LINE('',#5532,#1252);
#888=LINE('',#5538,#1253);
#889=LINE('',#5542,#1254);
#890=LINE('',#5544,#1255);
#891=LINE('',#5545,#1256);
#892=LINE('',#5550,#1257);
#893=LINE('',#5554,#1258);
#894=LINE('',#5556,#1259);
#895=LINE('',#5558,#1260);
#896=LINE('',#5560,#1261);
#897=LINE('',#5561,#1262);
#898=LINE('',#5562,#1263);
#899=LINE('',#5563,#1264);
#900=LINE('',#5564,#1265);
#901=LINE('',#5565,#1266);
#902=LINE('',#5566,#1267);
#903=LINE('',#5570,#1268);
#904=LINE('',#5573,#1269);
#905=LINE('',#5575,#1270);
#906=LINE('',#5576,#1271);
#907=LINE('',#5578,#1272);
#908=LINE('',#5579,#1273);
#909=LINE('',#5580,#1274);
#910=LINE('',#5583,#1275);
#911=LINE('',#5584,#1276);
#912=LINE('',#5586,#1277);
#913=LINE('',#5589,#1278);
#914=LINE('',#5591,#1279);
#915=LINE('',#5592,#1280);
#916=LINE('',#5596,#1281);
#917=LINE('',#5598,#1282);
#918=LINE('',#5599,#1283);
#919=LINE('',#5601,#1284);
#920=LINE('',#5602,#1285);
#921=LINE('',#5604,#1286);
#922=LINE('',#5608,#1287);
#923=LINE('',#5610,#1288);
#924=LINE('',#5611,#1289);
#925=LINE('',#5612,#1290);
#926=LINE('',#5614,#1291);
#927=LINE('',#5615,#1292);
#928=LINE('',#5617,#1293);
#929=LINE('',#5624,#1294);
#930=LINE('',#5625,#1295);
#931=LINE('',#5626,#1296);
#932=LINE('',#5627,#1297);
#933=LINE('',#5629,#1298);
#934=LINE('',#5631,#1299);
#935=LINE('',#5633,#1300);
#936=LINE('',#5636,#1301);
#937=LINE('',#5641,#1302);
#938=LINE('',#5643,#1303);
#939=LINE('',#5645,#1304);
#940=LINE('',#5647,#1305);
#941=LINE('',#5649,#1306);
#942=LINE('',#5650,#1307);
#943=LINE('',#5654,#1308);
#944=LINE('',#5656,#1309);
#945=LINE('',#5658,#1310);
#946=LINE('',#5660,#1311);
#947=LINE('',#5662,#1312);
#948=LINE('',#5663,#1313);
#949=LINE('',#5666,#1314);
#950=LINE('',#5668,#1315);
#951=LINE('',#5670,#1316);
#952=LINE('',#5671,#1317);
#953=LINE('',#5677,#1318);
#954=LINE('',#5681,#1319);
#955=LINE('',#5683,#1320);
#956=LINE('',#5685,#1321);
#957=LINE('',#5687,#1322);
#958=LINE('',#5688,#1323);
#959=LINE('',#5692,#1324);
#960=LINE('',#5694,#1325);
#961=LINE('',#5696,#1326);
#962=LINE('',#5697,#1327);
#963=LINE('',#5705,#1328);
#964=LINE('',#5708,#1329);
#965=LINE('',#5710,#1330);
#966=LINE('',#5711,#1331);
#967=LINE('',#5714,#1332);
#968=LINE('',#5716,#1333);
#969=LINE('',#5717,#1334);
#970=LINE('',#5720,#1335);
#971=LINE('',#5721,#1336);
#972=LINE('',#5724,#1337);
#973=LINE('',#5726,#1338);
#974=LINE('',#5727,#1339);
#975=LINE('',#5730,#1340);
#976=LINE('',#5731,#1341);
#977=LINE('',#5734,#1342);
#978=LINE('',#5738,#1343);
#979=LINE('',#5739,#1344);
#980=LINE('',#5743,#1345);
#981=LINE('',#5747,#1346);
#982=LINE('',#5750,#1347);
#983=LINE('',#5752,#1348);
#984=LINE('',#5754,#1349);
#985=LINE('',#5758,#1350);
#986=LINE('',#5762,#1351);
#987=LINE('',#5763,#1352);
#988=LINE('',#5766,#1353);
#989=LINE('',#5768,#1354);
#990=LINE('',#5770,#1355);
#991=LINE('',#5774,#1356);
#992=LINE('',#5775,#1357);
#993=LINE('',#5778,#1358);
#994=LINE('',#5779,#1359);
#995=LINE('',#5783,#1360);
#996=LINE('',#5786,#1361);
#997=LINE('',#5790,#1362);
#998=LINE('',#5793,#1363);
#999=LINE('',#5797,#1364);
#1000=LINE('',#5801,#1365);
#1001=LINE('',#5804,#1366);
#1002=LINE('',#5806,#1367);
#1003=LINE('',#5808,#1368);
#1004=LINE('',#5810,#1369);
#1005=LINE('',#5811,#1370);
#1006=LINE('',#5813,#1371);
#1007=LINE('',#5815,#1372);
#1008=LINE('',#5818,#1373);
#1009=LINE('',#5820,#1374);
#1010=LINE('',#5822,#1375);
#1011=LINE('',#5824,#1376);
#1012=LINE('',#5827,#1377);
#1013=LINE('',#5828,#1378);
#1014=LINE('',#5838,#1379);
#1015=LINE('',#5845,#1380);
#1016=LINE('',#5854,#1381);
#1017=LINE('',#5863,#1382);
#1018=LINE('',#5874,#1383);
#1019=LINE('',#5881,#1384);
#1020=VECTOR('',#3892,10.);
#1021=VECTOR('',#3899,2.);
#1022=VECTOR('',#3908,2.);
#1023=VECTOR('',#3919,2.);
#1024=VECTOR('',#3924,10.);
#1025=VECTOR('',#3925,10.);
#1026=VECTOR('',#3926,10.);
#1027=VECTOR('',#3927,10.);
#1028=VECTOR('',#3928,10.);
#1029=VECTOR('',#3933,1.50000013517123);
#1030=VECTOR('',#3942,1.4999996247669);
#1031=VECTOR('',#3949,10.);
#1032=VECTOR('',#3950,10.);
#1033=VECTOR('',#3951,10.);
#1034=VECTOR('',#3952,10.);
#1035=VECTOR('',#3953,10.);
#1036=VECTOR('',#3956,10.);
#1037=VECTOR('',#3957,10.);
#1038=VECTOR('',#3958,10.);
#1039=VECTOR('',#3959,10.);
#1040=VECTOR('',#3960,10.);
#1041=VECTOR('',#3961,10.);
#1042=VECTOR('',#3964,10.);
#1043=VECTOR('',#3965,10.);
#1044=VECTOR('',#3966,10.);
#1045=VECTOR('',#3967,10.);
#1046=VECTOR('',#3974,1.74999969554324);
#1047=VECTOR('',#3979,10.);
#1048=VECTOR('',#3980,10.);
#1049=VECTOR('',#3981,10.);
#1050=VECTOR('',#3982,10.);
#1051=VECTOR('',#3983,10.);
#1052=VECTOR('',#3986,10.);
#1053=VECTOR('',#3987,10.);
#1054=VECTOR('',#3988,10.);
#1055=VECTOR('',#3989,10.);
#1056=VECTOR('',#4002,10.);
#1057=VECTOR('',#4005,10.);
#1058=VECTOR('',#4006,10.);
#1059=VECTOR('',#4007,10.);
#1060=VECTOR('',#4010,10.);
#1061=VECTOR('',#4011,10.);
#1062=VECTOR('',#4012,10.);
#1063=VECTOR('',#4015,10.);
#1064=VECTOR('',#4016,10.);
#1065=VECTOR('',#4019,10.);
#1066=VECTOR('',#4020,10.);
#1067=VECTOR('',#4023,10.);
#1068=VECTOR('',#4024,10.);
#1069=VECTOR('',#4027,10.);
#1070=VECTOR('',#4028,10.);
#1071=VECTOR('',#4029,10.);
#1072=VECTOR('',#4032,10.);
#1073=VECTOR('',#4033,10.);
#1074=VECTOR('',#4038,10.);
#1075=VECTOR('',#4043,10.);
#1076=VECTOR('',#4044,10.);
#1077=VECTOR('',#4047,10.);
#1078=VECTOR('',#4050,10.);
#1079=VECTOR('',#4051,10.);
#1080=VECTOR('',#4054,10.);
#1081=VECTOR('',#4055,10.);
#1082=VECTOR('',#4056,10.);
#1083=VECTOR('',#4057,10.);
#1084=VECTOR('',#4064,10.);
#1085=VECTOR('',#4067,9.99999999999999);
#1086=VECTOR('',#4068,9.99999999999999);
#1087=VECTOR('',#4069,10.);
#1088=VECTOR('',#4078,10.);
#1089=VECTOR('',#4079,10.);
#1090=VECTOR('',#4080,10.);
#1091=VECTOR('',#4087,10.);
#1092=VECTOR('',#4090,10.);
#1093=VECTOR('',#4091,10.);
#1094=VECTOR('',#4092,10.);
#1095=VECTOR('',#4099,10.);
#1096=VECTOR('',#4102,10.);
#1097=VECTOR('',#4103,10.);
#1098=VECTOR('',#4104,10.);
#1099=VECTOR('',#4109,10.);
#1100=VECTOR('',#4116,10.);
#1101=VECTOR('',#4121,10.);
#1102=VECTOR('',#4124,10.);
#1103=VECTOR('',#4125,10.);
#1104=VECTOR('',#4126,10.);
#1105=VECTOR('',#4131,10.);
#1106=VECTOR('',#4136,10.);
#1107=VECTOR('',#4137,10.);
#1108=VECTOR('',#4138,10.);
#1109=VECTOR('',#4143,10.);
#1110=VECTOR('',#4148,9.99999999999999);
#1111=VECTOR('',#4149,10.);
#1112=VECTOR('',#4150,9.99999999999999);
#1113=VECTOR('',#4151,10.);
#1114=VECTOR('',#4156,10.);
#1115=VECTOR('',#4161,10.);
#1116=VECTOR('',#4164,10.);
#1117=VECTOR('',#4167,10.);
#1118=VECTOR('',#4168,10.);
#1119=VECTOR('',#4169,10.);
#1120=VECTOR('',#4170,10.);
#1121=VECTOR('',#4173,10.);
#1122=VECTOR('',#4174,10.);
#1123=VECTOR('',#4175,10.);
#1124=VECTOR('',#4176,10.);
#1125=VECTOR('',#4179,10.);
#1126=VECTOR('',#4180,10.);
#1127=VECTOR('',#4181,10.);
#1128=VECTOR('',#4182,10.);
#1129=VECTOR('',#4183,10.);
#1130=VECTOR('',#4184,10.);
#1131=VECTOR('',#4187,10.);
#1132=VECTOR('',#4188,10.);
#1133=VECTOR('',#4189,10.);
#1134=VECTOR('',#4190,10.);
#1135=VECTOR('',#4191,10.);
#1136=VECTOR('',#4192,10.);
#1137=VECTOR('',#4195,10.);
#1138=VECTOR('',#4196,10.);
#1139=VECTOR('',#4201,10.);
#1140=VECTOR('',#4206,10.);
#1141=VECTOR('',#4207,10.);
#1142=VECTOR('',#4208,10.);
#1143=VECTOR('',#4213,10.);
#1144=VECTOR('',#4216,10.);
#1145=VECTOR('',#4219,10.);
#1146=VECTOR('',#4220,10.);
#1147=VECTOR('',#4221,10.);
#1148=VECTOR('',#4222,10.);
#1149=VECTOR('',#4223,10.);
#1150=VECTOR('',#4224,10.);
#1151=VECTOR('',#4225,10.);
#1152=VECTOR('',#4230,10.);
#1153=VECTOR('',#4233,10.);
#1154=VECTOR('',#4236,10.);
#1155=VECTOR('',#4237,10.);
#1156=VECTOR('',#4238,10.);
#1157=VECTOR('',#4241,10.);
#1158=VECTOR('',#4244,10.);
#1159=VECTOR('',#4249,1.75000228959638);
#1160=VECTOR('',#4256,10.);
#1161=VECTOR('',#4257,10.);
#1162=VECTOR('',#4258,10.);
#1163=VECTOR('',#4259,10.);
#1164=VECTOR('',#4262,10.);
#1165=VECTOR('',#4263,10.);
#1166=VECTOR('',#4264,10.);
#1167=VECTOR('',#4265,10.);
#1168=VECTOR('',#4268,10.);
#1169=VECTOR('',#4269,10.);
#1170=VECTOR('',#4272,10.);
#1171=VECTOR('',#4275,10.);
#1172=VECTOR('',#4276,10.);
#1173=VECTOR('',#4277,10.);
#1174=VECTOR('',#4280,10.);
#1175=VECTOR('',#4283,10.);
#1176=VECTOR('',#4284,10.);
#1177=VECTOR('',#4287,10.);
#1178=VECTOR('',#4288,10.);
#1179=VECTOR('',#4291,10.);
#1180=VECTOR('',#4296,10.);
#1181=VECTOR('',#4297,10.);
#1182=VECTOR('',#4298,10.);
#1183=VECTOR('',#4299,10.);
#1184=VECTOR('',#4300,10.);
#1185=VECTOR('',#4301,10.);
#1186=VECTOR('',#4306,10.);
#1187=VECTOR('',#4311,10.);
#1188=VECTOR('',#4312,10.);
#1189=VECTOR('',#4313,10.);
#1190=VECTOR('',#4314,10.);
#1191=VECTOR('',#4315,10.);
#1192=VECTOR('',#4318,10.);
#1193=VECTOR('',#4321,10.);
#1194=VECTOR('',#4324,10.);
#1195=VECTOR('',#4327,10.);
#1196=VECTOR('',#4330,10.);
#1197=VECTOR('',#4333,10.);
#1198=VECTOR('',#4336,10.);
#1199=VECTOR('',#4343,10.);
#1200=VECTOR('',#4354,2.);
#1201=VECTOR('',#4363,2.);
#1202=VECTOR('',#4372,10.);
#1203=VECTOR('',#4373,10.);
#1204=VECTOR('',#4374,10.);
#1205=VECTOR('',#4375,10.);
#1206=VECTOR('',#4376,10.);
#1207=VECTOR('',#4379,10.);
#1208=VECTOR('',#4380,10.);
#1209=VECTOR('',#4381,10.);
#1210=VECTOR('',#4382,10.);
#1211=VECTOR('',#4383,10.);
#1212=VECTOR('',#4388,2.);
#1213=VECTOR('',#4395,1.50000013517123);
#1214=VECTOR('',#4404,1.4999996247669);
#1215=VECTOR('',#4411,10.);
#1216=VECTOR('',#4412,10.);
#1217=VECTOR('',#4413,10.);
#1218=VECTOR('',#4414,10.);
#1219=VECTOR('',#4419,10.);
#1220=VECTOR('',#4422,10.);
#1221=VECTOR('',#4427,10.);
#1222=VECTOR('',#4430,10.);
#1223=VECTOR('',#4433,10.);
#1224=VECTOR('',#4434,10.);
#1225=VECTOR('',#4435,10.);
#1226=VECTOR('',#4440,1.75000228959638);
#1227=VECTOR('',#4447,10.);
#1228=VECTOR('',#4448,10.);
#1229=VECTOR('',#4449,10.);
#1230=VECTOR('',#4450,10.);
#1231=VECTOR('',#4453,10.);
#1232=VECTOR('',#4454,10.);
#1233=VECTOR('',#4455,10.);
#1234=VECTOR('',#4456,10.);
#1235=VECTOR('',#4459,10.);
#1236=VECTOR('',#4460,10.);
#1237=VECTOR('',#4461,10.);
#1238=VECTOR('',#4462,10.);
#1239=VECTOR('',#4463,10.);
#1240=VECTOR('',#4466,10.);
#1241=VECTOR('',#4467,10.);
#1242=VECTOR('',#4468,10.);
#1243=VECTOR('',#4469,10.);
#1244=VECTOR('',#4470,10.);
#1245=VECTOR('',#4475,10.);
#1246=VECTOR('',#4480,10.);
#1247=VECTOR('',#4485,10.);
#1248=VECTOR('',#4488,10.);
#1249=VECTOR('',#4491,10.);
#1250=VECTOR('',#4492,10.);
#1251=VECTOR('',#4493,10.);
#1252=VECTOR('',#4498,10.);
#1253=VECTOR('',#4505,10.);
#1254=VECTOR('',#4510,9.99999999999999);
#1255=VECTOR('',#4511,10.);
#1256=VECTOR('',#4512,9.99999999999999);
#1257=VECTOR('',#4517,10.);
#1258=VECTOR('',#4522,10.);
#1259=VECTOR('',#4523,10.);
#1260=VECTOR('',#4524,10.);
#1261=VECTOR('',#4525,10.);
#1262=VECTOR('',#4526,10.);
#1263=VECTOR('',#4527,10.);
#1264=VECTOR('',#4528,10.);
#1265=VECTOR('',#4529,10.);
#1266=VECTOR('',#4530,10.);
#1267=VECTOR('',#4531,10.);
#1268=VECTOR('',#4536,10.);
#1269=VECTOR('',#4539,10.);
#1270=VECTOR('',#4540,10.);
#1271=VECTOR('',#4541,10.);
#1272=VECTOR('',#4542,10.);
#1273=VECTOR('',#4543,10.);
#1274=VECTOR('',#4544,10.);
#1275=VECTOR('',#4547,10.);
#1276=VECTOR('',#4548,10.);
#1277=VECTOR('',#4551,10.);
#1278=VECTOR('',#4554,10.);
#1279=VECTOR('',#4555,10.);
#1280=VECTOR('',#4556,10.);
#1281=VECTOR('',#4559,10.);
#1282=VECTOR('',#4560,10.);
#1283=VECTOR('',#4561,10.);
#1284=VECTOR('',#4562,10.);
#1285=VECTOR('',#4563,10.);
#1286=VECTOR('',#4566,10.);
#1287=VECTOR('',#4569,10.);
#1288=VECTOR('',#4570,10.);
#1289=VECTOR('',#4571,10.);
#1290=VECTOR('',#4572,10.);
#1291=VECTOR('',#4575,10.);
#1292=VECTOR('',#4576,10.);
#1293=VECTOR('',#4579,10.);
#1294=VECTOR('',#4592,10.);
#1295=VECTOR('',#4593,10.);
#1296=VECTOR('',#4594,10.);
#1297=VECTOR('',#4595,10.);
#1298=VECTOR('',#4598,10.);
#1299=VECTOR('',#4601,10.);
#1300=VECTOR('',#4604,10.);
#1301=VECTOR('',#4609,10.);
#1302=VECTOR('',#4614,10.);
#1303=VECTOR('',#4615,10.);
#1304=VECTOR('',#4616,10.);
#1305=VECTOR('',#4617,10.);
#1306=VECTOR('',#4618,10.);
#1307=VECTOR('',#4619,10.);
#1308=VECTOR('',#4622,10.);
#1309=VECTOR('',#4623,10.);
#1310=VECTOR('',#4624,10.);
#1311=VECTOR('',#4625,10.);
#1312=VECTOR('',#4626,10.);
#1313=VECTOR('',#4627,10.);
#1314=VECTOR('',#4630,10.);
#1315=VECTOR('',#4631,10.);
#1316=VECTOR('',#4632,10.);
#1317=VECTOR('',#4633,10.);
#1318=VECTOR('',#4640,1.74999969554324);
#1319=VECTOR('',#4645,10.);
#1320=VECTOR('',#4646,10.);
#1321=VECTOR('',#4647,10.);
#1322=VECTOR('',#4648,10.);
#1323=VECTOR('',#4649,10.);
#1324=VECTOR('',#4652,10.);
#1325=VECTOR('',#4653,10.);
#1326=VECTOR('',#4654,10.);
#1327=VECTOR('',#4655,10.);
#1328=VECTOR('',#4668,10.);
#1329=VECTOR('',#4671,10.);
#1330=VECTOR('',#4672,10.);
#1331=VECTOR('',#4673,10.);
#1332=VECTOR('',#4676,10.);
#1333=VECTOR('',#4677,10.);
#1334=VECTOR('',#4678,10.);
#1335=VECTOR('',#4681,10.);
#1336=VECTOR('',#4682,10.);
#1337=VECTOR('',#4685,10.);
#1338=VECTOR('',#4686,10.);
#1339=VECTOR('',#4687,10.);
#1340=VECTOR('',#4690,10.);
#1341=VECTOR('',#4691,10.);
#1342=VECTOR('',#4694,10.);
#1343=VECTOR('',#4697,10.);
#1344=VECTOR('',#4698,10.);
#1345=VECTOR('',#4701,10.);
#1346=VECTOR('',#4704,10.);
#1347=VECTOR('',#4707,10.);
#1348=VECTOR('',#4708,10.);
#1349=VECTOR('',#4709,10.);
#1350=VECTOR('',#4712,9.99999999999999);
#1351=VECTOR('',#4717,10.);
#1352=VECTOR('',#4718,10.);
#1353=VECTOR('',#4721,10.);
#1354=VECTOR('',#4722,10.);
#1355=VECTOR('',#4723,10.);
#1356=VECTOR('',#4726,10.);
#1357=VECTOR('',#4727,10.);
#1358=VECTOR('',#4730,10.);
#1359=VECTOR('',#4731,10.);
#1360=VECTOR('',#4736,10.);
#1361=VECTOR('',#4739,10.);
#1362=VECTOR('',#4742,10.);
#1363=VECTOR('',#4745,10.);
#1364=VECTOR('',#4748,9.99999999999999);
#1365=VECTOR('',#4751,10.);
#1366=VECTOR('',#4756,10.);
#1367=VECTOR('',#4759,10.);
#1368=VECTOR('',#4762,10.);
#1369=VECTOR('',#4765,10.);
#1370=VECTOR('',#4766,10.);
#1371=VECTOR('',#4769,10.);
#1372=VECTOR('',#4772,10.);
#1373=VECTOR('',#4777,10.);
#1374=VECTOR('',#4780,10.);
#1375=VECTOR('',#4783,10.);
#1376=VECTOR('',#4786,10.);
#1377=VECTOR('',#4789,10.);
#1378=VECTOR('',#4790,10.);
#1379=VECTOR('',#4805,1.50000013517123);
#1380=VECTOR('',#4814,1.4999996247669);
#1381=VECTOR('',#4827,1.50000013517123);
#1382=VECTOR('',#4840,2.);
#1383=VECTOR('',#4857,1.4999996247669);
#1384=VECTOR('',#4866,2.);
#1385=VERTEX_POINT('',#4892);
#1386=VERTEX_POINT('',#4893);
#1387=VERTEX_POINT('',#4897);
#1388=VERTEX_POINT('',#4899);
#1389=VERTEX_POINT('',#4904);
#1390=VERTEX_POINT('',#4906);
#1391=VERTEX_POINT('',#4910);
#1392=VERTEX_POINT('',#4911);
#1393=VERTEX_POINT('',#4913);
#1394=VERTEX_POINT('',#4916);
#1395=VERTEX_POINT('',#4920);
#1396=VERTEX_POINT('',#4922);
#1397=VERTEX_POINT('',#4924);
#1398=VERTEX_POINT('',#4926);
#1399=VERTEX_POINT('',#4930);
#1400=VERTEX_POINT('',#4932);
#1401=VERTEX_POINT('',#4937);
#1402=VERTEX_POINT('',#4939);
#1403=VERTEX_POINT('',#4944);
#1404=VERTEX_POINT('',#4946);
#1405=VERTEX_POINT('',#4948);
#1406=VERTEX_POINT('',#4950);
#1407=VERTEX_POINT('',#4954);
#1408=VERTEX_POINT('',#4955);
#1409=VERTEX_POINT('',#4957);
#1410=VERTEX_POINT('',#4959);
#1411=VERTEX_POINT('',#4961);
#1412=VERTEX_POINT('',#4963);
#1413=VERTEX_POINT('',#4967);
#1414=VERTEX_POINT('',#4969);
#1415=VERTEX_POINT('',#4971);
#1416=VERTEX_POINT('',#4975);
#1417=VERTEX_POINT('',#4978);
#1418=VERTEX_POINT('',#4982);
#1419=VERTEX_POINT('',#4984);
#1420=VERTEX_POINT('',#4986);
#1421=VERTEX_POINT('',#4988);
#1422=VERTEX_POINT('',#4992);
#1423=VERTEX_POINT('',#4993);
#1424=VERTEX_POINT('',#4995);
#1425=VERTEX_POINT('',#4997);
#1426=VERTEX_POINT('',#5004);
#1427=VERTEX_POINT('',#5009);
#1428=VERTEX_POINT('',#5011);
#1429=VERTEX_POINT('',#5015);
#1430=VERTEX_POINT('',#5017);
#1431=VERTEX_POINT('',#5021);
#1432=VERTEX_POINT('',#5025);
#1433=VERTEX_POINT('',#5029);
#1434=VERTEX_POINT('',#5033);
#1435=VERTEX_POINT('',#5035);
#1436=VERTEX_POINT('',#5037);
#1437=VERTEX_POINT('',#5039);
#1438=VERTEX_POINT('',#5041);
#1439=VERTEX_POINT('',#5045);
#1440=VERTEX_POINT('',#5047);
#1441=VERTEX_POINT('',#5051);
#1442=VERTEX_POINT('',#5057);
#1443=VERTEX_POINT('',#5061);
#1444=VERTEX_POINT('',#5063);
#1445=VERTEX_POINT('',#5065);
#1446=VERTEX_POINT('',#5069);
#1447=VERTEX_POINT('',#5071);
#1448=VERTEX_POINT('',#5075);
#1449=VERTEX_POINT('',#5077);
#1450=VERTEX_POINT('',#5084);
#1451=VERTEX_POINT('',#5086);
#1452=VERTEX_POINT('',#5090);
#1453=VERTEX_POINT('',#5092);
#1454=VERTEX_POINT('',#5096);
#1455=VERTEX_POINT('',#5098);
#1456=VERTEX_POINT('',#5102);
#1457=VERTEX_POINT('',#5104);
#1458=VERTEX_POINT('',#5108);
#1459=VERTEX_POINT('',#5110);
#1460=VERTEX_POINT('',#5114);
#1461=VERTEX_POINT('',#5116);
#1462=VERTEX_POINT('',#5120);
#1463=VERTEX_POINT('',#5121);
#1464=VERTEX_POINT('',#5123);
#1465=VERTEX_POINT('',#5125);
#1466=VERTEX_POINT('',#5127);
#1467=VERTEX_POINT('',#5131);
#1468=VERTEX_POINT('',#5133);
#1469=VERTEX_POINT('',#5137);
#1470=VERTEX_POINT('',#5139);
#1471=VERTEX_POINT('',#5143);
#1472=VERTEX_POINT('',#5145);
#1473=VERTEX_POINT('',#5149);
#1474=VERTEX_POINT('',#5151);
#1475=VERTEX_POINT('',#5155);
#1476=VERTEX_POINT('',#5156);
#1477=VERTEX_POINT('',#5158);
#1478=VERTEX_POINT('',#5160);
#1479=VERTEX_POINT('',#5164);
#1480=VERTEX_POINT('',#5166);
#1481=VERTEX_POINT('',#5170);
#1482=VERTEX_POINT('',#5172);
#1483=VERTEX_POINT('',#5176);
#1484=VERTEX_POINT('',#5177);
#1485=VERTEX_POINT('',#5179);
#1486=VERTEX_POINT('',#5181);
#1487=VERTEX_POINT('',#5185);
#1488=VERTEX_POINT('',#5186);
#1489=VERTEX_POINT('',#5188);
#1490=VERTEX_POINT('',#5190);
#1491=VERTEX_POINT('',#5194);
#1492=VERTEX_POINT('',#5195);
#1493=VERTEX_POINT('',#5197);
#1494=VERTEX_POINT('',#5199);
#1495=VERTEX_POINT('',#5201);
#1496=VERTEX_POINT('',#5203);
#1497=VERTEX_POINT('',#5207);
#1498=VERTEX_POINT('',#5208);
#1499=VERTEX_POINT('',#5210);
#1500=VERTEX_POINT('',#5212);
#1501=VERTEX_POINT('',#5214);
#1502=VERTEX_POINT('',#5216);
#1503=VERTEX_POINT('',#5223);
#1504=VERTEX_POINT('',#5225);
#1505=VERTEX_POINT('',#5229);
#1506=VERTEX_POINT('',#5231);
#1507=VERTEX_POINT('',#5235);
#1508=VERTEX_POINT('',#5237);
#1509=VERTEX_POINT('',#5239);
#1510=VERTEX_POINT('',#5243);
#1511=VERTEX_POINT('',#5245);
#1512=VERTEX_POINT('',#5247);
#1513=VERTEX_POINT('',#5254);
#1514=VERTEX_POINT('',#5255);
#1515=VERTEX_POINT('',#5257);
#1516=VERTEX_POINT('',#5259);
#1517=VERTEX_POINT('',#5263);
#1518=VERTEX_POINT('',#5265);
#1519=VERTEX_POINT('',#5273);
#1520=VERTEX_POINT('',#5275);
#1521=VERTEX_POINT('',#5280);
#1522=VERTEX_POINT('',#5281);
#1523=VERTEX_POINT('',#5283);
#1524=VERTEX_POINT('',#5285);
#1525=VERTEX_POINT('',#5289);
#1526=VERTEX_POINT('',#5292);
#1527=VERTEX_POINT('',#5296);
#1528=VERTEX_POINT('',#5302);
#1529=VERTEX_POINT('',#5304);
#1530=VERTEX_POINT('',#5310);
#1531=VERTEX_POINT('',#5314);
#1532=VERTEX_POINT('',#5321);
#1533=VERTEX_POINT('',#5322);
#1534=VERTEX_POINT('',#5324);
#1535=VERTEX_POINT('',#5326);
#1536=VERTEX_POINT('',#5328);
#1537=VERTEX_POINT('',#5330);
#1538=VERTEX_POINT('',#5360);
#1539=VERTEX_POINT('',#5361);
#1540=VERTEX_POINT('',#5365);
#1541=VERTEX_POINT('',#5366);
#1542=VERTEX_POINT('',#5368);
#1543=VERTEX_POINT('',#5371);
#1544=VERTEX_POINT('',#5376);
#1545=VERTEX_POINT('',#5378);
#1546=VERTEX_POINT('',#5380);
#1547=VERTEX_POINT('',#5382);
#1548=VERTEX_POINT('',#5386);
#1549=VERTEX_POINT('',#5388);
#1550=VERTEX_POINT('',#5390);
#1551=VERTEX_POINT('',#5392);
#1552=VERTEX_POINT('',#5396);
#1553=VERTEX_POINT('',#5398);
#1554=VERTEX_POINT('',#5400);
#1555=VERTEX_POINT('',#5402);
#1556=VERTEX_POINT('',#5406);
#1557=VERTEX_POINT('',#5408);
#1558=VERTEX_POINT('',#5412);
#1559=VERTEX_POINT('',#5414);
#1560=VERTEX_POINT('',#5419);
#1561=VERTEX_POINT('',#5421);
#1562=VERTEX_POINT('',#5426);
#1563=VERTEX_POINT('',#5427);
#1564=VERTEX_POINT('',#5429);
#1565=VERTEX_POINT('',#5431);
#1566=VERTEX_POINT('',#5435);
#1567=VERTEX_POINT('',#5437);
#1568=VERTEX_POINT('',#5439);
#1569=VERTEX_POINT('',#5443);
#1570=VERTEX_POINT('',#5444);
#1571=VERTEX_POINT('',#5446);
#1572=VERTEX_POINT('',#5448);
#1573=VERTEX_POINT('',#5452);
#1574=VERTEX_POINT('',#5454);
#1575=VERTEX_POINT('',#5458);
#1576=VERTEX_POINT('',#5460);
#1577=VERTEX_POINT('',#5465);
#1578=VERTEX_POINT('',#5466);
#1579=VERTEX_POINT('',#5468);
#1580=VERTEX_POINT('',#5470);
#1581=VERTEX_POINT('',#5474);
#1582=VERTEX_POINT('',#5475);
#1583=VERTEX_POINT('',#5477);
#1584=VERTEX_POINT('',#5479);
#1585=VERTEX_POINT('',#5483);
#1586=VERTEX_POINT('',#5484);
#1587=VERTEX_POINT('',#5486);
#1588=VERTEX_POINT('',#5489);
#1589=VERTEX_POINT('',#5493);
#1590=VERTEX_POINT('',#5494);
#1591=VERTEX_POINT('',#5496);
#1592=VERTEX_POINT('',#5499);
#1593=VERTEX_POINT('',#5503);
#1594=VERTEX_POINT('',#5504);
#1595=VERTEX_POINT('',#5506);
#1596=VERTEX_POINT('',#5508);
#1597=VERTEX_POINT('',#5510);
#1598=VERTEX_POINT('',#5514);
#1599=VERTEX_POINT('',#5515);
#1600=VERTEX_POINT('',#5517);
#1601=VERTEX_POINT('',#5519);
#1602=VERTEX_POINT('',#5523);
#1603=VERTEX_POINT('',#5525);
#1604=VERTEX_POINT('',#5529);
#1605=VERTEX_POINT('',#5531);
#1606=VERTEX_POINT('',#5535);
#1607=VERTEX_POINT('',#5537);
#1608=VERTEX_POINT('',#5541);
#1609=VERTEX_POINT('',#5543);
#1610=VERTEX_POINT('',#5547);
#1611=VERTEX_POINT('',#5549);
#1612=VERTEX_POINT('',#5553);
#1613=VERTEX_POINT('',#5555);
#1614=VERTEX_POINT('',#5557);
#1615=VERTEX_POINT('',#5559);
#1616=VERTEX_POINT('',#5568);
#1617=VERTEX_POINT('',#5572);
#1618=VERTEX_POINT('',#5574);
#1619=VERTEX_POINT('',#5577);
#1620=VERTEX_POINT('',#5582);
#1621=VERTEX_POINT('',#5588);
#1622=VERTEX_POINT('',#5590);
#1623=VERTEX_POINT('',#5594);
#1624=VERTEX_POINT('',#5595);
#1625=VERTEX_POINT('',#5597);
#1626=VERTEX_POINT('',#5600);
#1627=VERTEX_POINT('',#5606);
#1628=VERTEX_POINT('',#5607);
#1629=VERTEX_POINT('',#5609);
#1630=VERTEX_POINT('',#5639);
#1631=VERTEX_POINT('',#5640);
#1632=VERTEX_POINT('',#5642);
#1633=VERTEX_POINT('',#5644);
#1634=VERTEX_POINT('',#5646);
#1635=VERTEX_POINT('',#5648);
#1636=VERTEX_POINT('',#5652);
#1637=VERTEX_POINT('',#5653);
#1638=VERTEX_POINT('',#5655);
#1639=VERTEX_POINT('',#5657);
#1640=VERTEX_POINT('',#5659);
#1641=VERTEX_POINT('',#5661);
#1642=VERTEX_POINT('',#5665);
#1643=VERTEX_POINT('',#5667);
#1644=VERTEX_POINT('',#5669);
#1645=VERTEX_POINT('',#5673);
#1646=VERTEX_POINT('',#5676);
#1647=VERTEX_POINT('',#5680);
#1648=VERTEX_POINT('',#5682);
#1649=VERTEX_POINT('',#5684);
#1650=VERTEX_POINT('',#5686);
#1651=VERTEX_POINT('',#5690);
#1652=VERTEX_POINT('',#5691);
#1653=VERTEX_POINT('',#5693);
#1654=VERTEX_POINT('',#5695);
#1655=VERTEX_POINT('',#5702);
#1656=VERTEX_POINT('',#5707);
#1657=VERTEX_POINT('',#5709);
#1658=VERTEX_POINT('',#5713);
#1659=VERTEX_POINT('',#5715);
#1660=VERTEX_POINT('',#5719);
#1661=VERTEX_POINT('',#5723);
#1662=VERTEX_POINT('',#5725);
#1663=VERTEX_POINT('',#5729);
#1664=VERTEX_POINT('',#5733);
#1665=VERTEX_POINT('',#5735);
#1666=VERTEX_POINT('',#5737);
#1667=VERTEX_POINT('',#5740);
#1668=VERTEX_POINT('',#5742);
#1669=VERTEX_POINT('',#5744);
#1670=VERTEX_POINT('',#5746);
#1671=VERTEX_POINT('',#5748);
#1672=VERTEX_POINT('',#5751);
#1673=VERTEX_POINT('',#5753);
#1674=VERTEX_POINT('',#5755);
#1675=VERTEX_POINT('',#5757);
#1676=VERTEX_POINT('',#5761);
#1677=VERTEX_POINT('',#5765);
#1678=VERTEX_POINT('',#5767);
#1679=VERTEX_POINT('',#5769);
#1680=VERTEX_POINT('',#5771);
#1681=VERTEX_POINT('',#5773);
#1682=VERTEX_POINT('',#5777);
#1683=VERTEX_POINT('',#5781);
#1684=VERTEX_POINT('',#5785);
#1685=VERTEX_POINT('',#5787);
#1686=VERTEX_POINT('',#5789);
#1687=VERTEX_POINT('',#5791);
#1688=VERTEX_POINT('',#5794);
#1689=VERTEX_POINT('',#5796);
#1690=VERTEX_POINT('',#5798);
#1691=VERTEX_POINT('',#5800);
#1692=VERTEX_POINT('',#5826);
#1693=VERTEX_POINT('',#5833);
#1694=VERTEX_POINT('',#5836);
#1695=VERTEX_POINT('',#5842);
#1696=VERTEX_POINT('',#5844);
#1697=VERTEX_POINT('',#5851);
#1698=VERTEX_POINT('',#5853);
#1699=VERTEX_POINT('',#5860);
#1700=VERTEX_POINT('',#5862);
#1701=VERTEX_POINT('',#5869);
#1702=VERTEX_POINT('',#5872);
#1703=VERTEX_POINT('',#5878);
#1704=VERTEX_POINT('',#5880);
#1705=EDGE_CURVE('',#1385,#1386,#655,.T.);
#1706=EDGE_CURVE('',#1386,#1385,#553,.T.);
#1707=EDGE_CURVE('',#1387,#1387,#96,.T.);
#1708=EDGE_CURVE('',#1387,#1388,#656,.T.);
#1709=EDGE_CURVE('',#1386,#1388,#97,.T.);
#1710=EDGE_CURVE('',#1388,#1385,#98,.T.);
#1711=EDGE_CURVE('',#1389,#1389,#554,.T.);
#1712=EDGE_CURVE('',#1389,#1390,#657,.T.);
#1713=EDGE_CURVE('',#1390,#1390,#99,.T.);
#1714=EDGE_CURVE('',#1391,#1392,#100,.T.);
#1715=EDGE_CURVE('',#1393,#1391,#101,.T.);
#1716=EDGE_CURVE('',#1392,#1393,#102,.T.);
#1717=EDGE_CURVE('',#1392,#1394,#658,.T.);
#1718=EDGE_CURVE('',#1394,#1394,#103,.T.);
#1719=EDGE_CURVE('',#1393,#1395,#659,.T.);
#1720=EDGE_CURVE('',#1395,#1396,#660,.T.);
#1721=EDGE_CURVE('',#1397,#1396,#661,.T.);
#1722=EDGE_CURVE('',#1398,#1397,#662,.T.);
#1723=EDGE_CURVE('',#1398,#1391,#663,.T.);
#1724=EDGE_CURVE('',#1399,#1399,#555,.T.);
#1725=EDGE_CURVE('',#1399,#1400,#664,.T.);
#1726=EDGE_CURVE('',#1400,#1400,#556,.T.);
#1727=EDGE_CURVE('',#1401,#1401,#557,.T.);
#1728=EDGE_CURVE('',#1401,#1402,#665,.T.);
#1729=EDGE_CURVE('',#1402,#1402,#558,.T.);
#1730=EDGE_CURVE('',#1396,#1403,#666,.T.);
#1731=EDGE_CURVE('',#1404,#1395,#667,.T.);
#1732=EDGE_CURVE('',#1405,#1404,#668,.T.);
#1733=EDGE_CURVE('',#1406,#1405,#669,.T.);
#1734=EDGE_CURVE('',#1403,#1406,#670,.T.);
#1735=EDGE_CURVE('',#1407,#1408,#671,.T.);
#1736=EDGE_CURVE('',#1409,#1407,#672,.T.);
#1737=EDGE_CURVE('',#1410,#1409,#673,.T.);
#1738=EDGE_CURVE('',#1411,#1410,#674,.T.);
#1739=EDGE_CURVE('',#1412,#1411,#675,.T.);
#1740=EDGE_CURVE('',#1412,#1408,#676,.T.);
#1741=EDGE_CURVE('',#1413,#1407,#677,.T.);
#1742=EDGE_CURVE('',#1414,#1413,#678,.T.);
#1743=EDGE_CURVE('',#1415,#1414,#679,.T.);
#1744=EDGE_CURVE('',#1415,#1409,#680,.T.);
#1745=EDGE_CURVE('',#1416,#1416,#559,.T.);
#1746=EDGE_CURVE('',#1416,#1417,#681,.T.);
#1747=EDGE_CURVE('',#1417,#1417,#560,.T.);
#1748=EDGE_CURVE('',#1418,#1406,#682,.T.);
#1749=EDGE_CURVE('',#1418,#1419,#683,.T.);
#1750=EDGE_CURVE('',#1420,#1419,#684,.T.);
#1751=EDGE_CURVE('',#1420,#1421,#685,.T.);
#1752=EDGE_CURVE('',#1403,#1421,#686,.T.);
#1753=EDGE_CURVE('',#1422,#1423,#687,.T.);
#1754=EDGE_CURVE('',#1422,#1424,#688,.T.);
#1755=EDGE_CURVE('',#1425,#1424,#689,.T.);
#1756=EDGE_CURVE('',#1423,#1425,#690,.T.);
#1757=EDGE_CURVE('',#1423,#1418,#561,.T.);
#1758=EDGE_CURVE('',#1419,#1425,#562,.T.);
#1759=EDGE_CURVE('',#1415,#1426,#563,.T.);
#1760=EDGE_CURVE('',#1421,#1413,#564,.T.);
#1761=EDGE_CURVE('',#1426,#1420,#691,.T.);
#1762=EDGE_CURVE('',#1427,#1426,#692,.T.);
#1763=EDGE_CURVE('',#1428,#1420,#693,.T.);
#1764=EDGE_CURVE('',#1427,#1428,#694,.T.);
#1765=EDGE_CURVE('',#1429,#1410,#695,.T.);
#1766=EDGE_CURVE('',#1429,#1430,#696,.T.);
#1767=EDGE_CURVE('',#1430,#1411,#697,.T.);
#1768=EDGE_CURVE('',#1430,#1431,#698,.T.);
#1769=EDGE_CURVE('',#1412,#1431,#699,.T.);
#1770=EDGE_CURVE('',#1398,#1432,#700,.T.);
#1771=EDGE_CURVE('',#1432,#1404,#701,.T.);
#1772=EDGE_CURVE('',#1432,#1433,#702,.T.);
#1773=EDGE_CURVE('',#1405,#1433,#703,.T.);
#1774=EDGE_CURVE('',#1408,#1434,#704,.T.);
#1775=EDGE_CURVE('',#1434,#1435,#705,.T.);
#1776=EDGE_CURVE('',#1435,#1436,#706,.T.);
#1777=EDGE_CURVE('',#1436,#1437,#565,.T.);
#1778=EDGE_CURVE('',#1437,#1438,#707,.T.);
#1779=EDGE_CURVE('',#1438,#1397,#708,.T.);
#1780=EDGE_CURVE('',#1439,#1428,#566,.T.);
#1781=EDGE_CURVE('',#1440,#1439,#709,.T.);
#1782=EDGE_CURVE('',#1427,#1440,#567,.T.);
#1783=EDGE_CURVE('',#1441,#1438,#710,.T.);
#1784=EDGE_CURVE('',#1433,#1441,#711,.T.);
#1785=EDGE_CURVE('',#1431,#1434,#712,.T.);
#1786=EDGE_CURVE('',#1442,#1429,#713,.T.);
#1787=EDGE_CURVE('',#1435,#1442,#714,.T.);
#1788=EDGE_CURVE('',#1443,#1437,#715,.T.);
#1789=EDGE_CURVE('',#1444,#1443,#716,.T.);
#1790=EDGE_CURVE('',#1445,#1444,#717,.T.);
#1791=EDGE_CURVE('',#1441,#1445,#718,.T.);
#1792=EDGE_CURVE('',#1445,#1446,#568,.T.);
#1793=EDGE_CURVE('',#1447,#1444,#569,.T.);
#1794=EDGE_CURVE('',#1446,#1447,#719,.T.);
#1795=EDGE_CURVE('',#1446,#1448,#720,.T.);
#1796=EDGE_CURVE('',#1449,#1447,#721,.T.);
#1797=EDGE_CURVE('',#1448,#1449,#722,.T.);
#1798=EDGE_CURVE('',#1448,#1422,#570,.T.);
#1799=EDGE_CURVE('',#1424,#1449,#571,.T.);
#1800=EDGE_CURVE('',#1440,#1450,#723,.T.);
#1801=EDGE_CURVE('',#1451,#1439,#724,.T.);
#1802=EDGE_CURVE('',#1450,#1451,#725,.T.);
#1803=EDGE_CURVE('',#1450,#1452,#572,.T.);
#1804=EDGE_CURVE('',#1453,#1451,#573,.T.);
#1805=EDGE_CURVE('',#1452,#1453,#726,.T.);
#1806=EDGE_CURVE('',#1454,#1452,#727,.T.);
#1807=EDGE_CURVE('',#1455,#1453,#728,.T.);
#1808=EDGE_CURVE('',#1454,#1455,#729,.T.);
#1809=EDGE_CURVE('',#1456,#1454,#574,.T.);
#1810=EDGE_CURVE('',#1457,#1455,#575,.T.);
#1811=EDGE_CURVE('',#1457,#1456,#730,.T.);
#1812=EDGE_CURVE('',#1442,#1458,#731,.T.);
#1813=EDGE_CURVE('',#1458,#1459,#732,.T.);
#1814=EDGE_CURVE('',#1459,#1436,#733,.T.);
#1815=EDGE_CURVE('',#1460,#1458,#576,.T.);
#1816=EDGE_CURVE('',#1460,#1461,#734,.T.);
#1817=EDGE_CURVE('',#1443,#1461,#577,.T.);
#1818=EDGE_CURVE('',#1462,#1463,#578,.T.);
#1819=EDGE_CURVE('',#1462,#1464,#735,.T.);
#1820=EDGE_CURVE('',#1465,#1464,#579,.T.);
#1821=EDGE_CURVE('',#1466,#1465,#580,.T.);
#1822=EDGE_CURVE('',#1463,#1466,#736,.T.);
#1823=EDGE_CURVE('',#1467,#1460,#737,.T.);
#1824=EDGE_CURVE('',#1467,#1468,#738,.T.);
#1825=EDGE_CURVE('',#1461,#1468,#739,.T.);
#1826=EDGE_CURVE('',#1467,#1469,#581,.T.);
#1827=EDGE_CURVE('',#1469,#1470,#740,.T.);
#1828=EDGE_CURVE('',#1468,#1470,#582,.T.);
#1829=EDGE_CURVE('',#1469,#1471,#741,.T.);
#1830=EDGE_CURVE('',#1471,#1472,#742,.T.);
#1831=EDGE_CURVE('',#1470,#1472,#743,.T.);
#1832=EDGE_CURVE('',#1473,#1471,#583,.T.);
#1833=EDGE_CURVE('',#1473,#1474,#744,.T.);
#1834=EDGE_CURVE('',#1472,#1474,#584,.T.);
#1835=EDGE_CURVE('',#1475,#1476,#745,.T.);
#1836=EDGE_CURVE('',#1475,#1477,#746,.T.);
#1837=EDGE_CURVE('',#1478,#1477,#747,.T.);
#1838=EDGE_CURVE('',#1476,#1478,#748,.T.);
#1839=EDGE_CURVE('',#1479,#1475,#585,.T.);
#1840=EDGE_CURVE('',#1479,#1480,#749,.T.);
#1841=EDGE_CURVE('',#1477,#1480,#586,.T.);
#1842=EDGE_CURVE('',#1465,#1481,#750,.T.);
#1843=EDGE_CURVE('',#1482,#1481,#587,.T.);
#1844=EDGE_CURVE('',#1466,#1482,#751,.T.);
#1845=EDGE_CURVE('',#1483,#1484,#752,.T.);
#1846=EDGE_CURVE('',#1485,#1483,#753,.T.);
#1847=EDGE_CURVE('',#1485,#1486,#754,.T.);
#1848=EDGE_CURVE('',#1484,#1486,#755,.T.);
#1849=EDGE_CURVE('',#1487,#1488,#756,.T.);
#1850=EDGE_CURVE('',#1487,#1489,#757,.T.);
#1851=EDGE_CURVE('',#1489,#1490,#758,.T.);
#1852=EDGE_CURVE('',#1488,#1490,#759,.T.);
#1853=EDGE_CURVE('',#1491,#1492,#760,.T.);
#1854=EDGE_CURVE('',#1492,#1493,#761,.T.);
#1855=EDGE_CURVE('',#1494,#1493,#762,.T.);
#1856=EDGE_CURVE('',#1494,#1495,#763,.T.);
#1857=EDGE_CURVE('',#1495,#1496,#764,.T.);
#1858=EDGE_CURVE('',#1496,#1491,#765,.T.);
#1859=EDGE_CURVE('',#1497,#1498,#766,.T.);
#1860=EDGE_CURVE('',#1498,#1499,#767,.T.);
#1861=EDGE_CURVE('',#1499,#1500,#768,.T.);
#1862=EDGE_CURVE('',#1500,#1501,#769,.T.);
#1863=EDGE_CURVE('',#1502,#1501,#770,.T.);
#1864=EDGE_CURVE('',#1502,#1497,#771,.T.);
#1865=EDGE_CURVE('',#1464,#1457,#772,.T.);
#1866=EDGE_CURVE('',#1462,#1456,#773,.T.);
#1867=EDGE_CURVE('',#1503,#1473,#588,.T.);
#1868=EDGE_CURVE('',#1503,#1504,#774,.T.);
#1869=EDGE_CURVE('',#1474,#1504,#589,.T.);
#1870=EDGE_CURVE('',#1505,#1503,#775,.T.);
#1871=EDGE_CURVE('',#1505,#1506,#776,.T.);
#1872=EDGE_CURVE('',#1504,#1506,#777,.T.);
#1873=EDGE_CURVE('',#1507,#1505,#590,.T.);
#1874=EDGE_CURVE('',#1507,#1508,#778,.T.);
#1875=EDGE_CURVE('',#1509,#1508,#591,.T.);
#1876=EDGE_CURVE('',#1506,#1509,#779,.T.);
#1877=EDGE_CURVE('',#1493,#1510,#780,.T.);
#1878=EDGE_CURVE('',#1510,#1511,#781,.T.);
#1879=EDGE_CURVE('',#1511,#1512,#782,.T.);
#1880=EDGE_CURVE('',#1508,#1512,#783,.T.);
#1881=EDGE_CURVE('',#1507,#1463,#784,.T.);
#1882=EDGE_CURVE('',#1488,#1482,#785,.T.);
#1883=EDGE_CURVE('',#1490,#1493,#786,.T.);
#1884=EDGE_CURVE('',#1513,#1514,#592,.T.);
#1885=EDGE_CURVE('',#1513,#1515,#787,.T.);
#1886=EDGE_CURVE('',#1516,#1515,#593,.T.);
#1887=EDGE_CURVE('',#1514,#1516,#788,.T.);
#1888=EDGE_CURVE('',#1517,#1513,#789,.T.);
#1889=EDGE_CURVE('',#1517,#1518,#790,.T.);
#1890=EDGE_CURVE('',#1515,#1518,#791,.T.);
#1891=EDGE_CURVE('',#1506,#1516,#792,.T.);
#1892=EDGE_CURVE('',#1518,#1478,#594,.T.);
#1893=EDGE_CURVE('',#1480,#1465,#793,.T.);
#1894=EDGE_CURVE('',#1519,#1519,#595,.T.);
#1895=EDGE_CURVE('',#1519,#1520,#794,.T.);
#1896=EDGE_CURVE('',#1520,#1520,#596,.T.);
#1897=EDGE_CURVE('',#1521,#1522,#795,.T.);
#1898=EDGE_CURVE('',#1521,#1523,#796,.T.);
#1899=EDGE_CURVE('',#1523,#1524,#797,.T.);
#1900=EDGE_CURVE('',#1522,#1524,#798,.T.);
#1901=EDGE_CURVE('',#1525,#1489,#799,.T.);
#1902=EDGE_CURVE('',#1511,#1525,#800,.T.);
#1903=EDGE_CURVE('',#1510,#1526,#801,.T.);
#1904=EDGE_CURVE('',#1526,#1494,#802,.T.);
#1905=EDGE_CURVE('',#1512,#1527,#803,.T.);
#1906=EDGE_CURVE('',#1527,#1525,#804,.T.);
#1907=EDGE_CURVE('',#1527,#1487,#805,.T.);
#1908=EDGE_CURVE('',#1491,#1528,#806,.T.);
#1909=EDGE_CURVE('',#1529,#1528,#807,.T.);
#1910=EDGE_CURVE('',#1529,#1492,#808,.T.);
#1911=EDGE_CURVE('',#1510,#1529,#809,.T.);
#1912=EDGE_CURVE('',#1530,#1526,#810,.T.);
#1913=EDGE_CURVE('',#1530,#1495,#811,.T.);
#1914=EDGE_CURVE('',#1531,#1530,#812,.T.);
#1915=EDGE_CURVE('',#1531,#1496,#813,.T.);
#1916=EDGE_CURVE('',#1528,#1531,#814,.T.);
#1917=EDGE_CURVE('',#1532,#1533,#815,.T.);
#1918=EDGE_CURVE('',#1533,#1534,#816,.T.);
#1919=EDGE_CURVE('',#1535,#1534,#817,.T.);
#1920=EDGE_CURVE('',#1535,#1536,#818,.T.);
#1921=EDGE_CURVE('',#1536,#1537,#819,.T.);
#1922=EDGE_CURVE('',#1537,#1532,#820,.T.);
#1923=EDGE_CURVE('',#1476,#1517,#597,.T.);
#1924=EDGE_CURVE('',#1514,#1479,#821,.T.);
#1925=EDGE_CURVE('',#1522,#1509,#822,.T.);
#1926=EDGE_CURVE('',#1524,#1534,#823,.T.);
#1927=EDGE_CURVE('',#1534,#1502,#824,.T.);
#1928=EDGE_CURVE('',#1502,#1485,#825,.T.);
#1929=EDGE_CURVE('',#1481,#1483,#826,.T.);
#1930=EDGE_CURVE('',#1497,#1533,#827,.T.);
#1931=EDGE_CURVE('',#1532,#1498,#828,.T.);
#1932=EDGE_CURVE('',#1537,#1499,#829,.T.);
#1933=EDGE_CURVE('',#1536,#1500,#830,.T.);
#1934=EDGE_CURVE('',#1501,#1535,#831,.T.);
#1935=EDGE_CURVE('',#1486,#1523,#832,.T.);
#1936=EDGE_CURVE('',#1484,#1521,#833,.T.);
#1937=EDGE_CURVE('',#1538,#1539,#834,.T.);
#1938=EDGE_CURVE('',#1538,#1539,#598,.T.);
#1939=EDGE_CURVE('',#1540,#1541,#104,.T.);
#1940=EDGE_CURVE('',#1542,#1540,#105,.T.);
#1941=EDGE_CURVE('',#1541,#1542,#106,.T.);
#1942=EDGE_CURVE('',#1541,#1543,#835,.T.);
#1943=EDGE_CURVE('',#1539,#1543,#107,.T.);
#1944=EDGE_CURVE('',#1543,#1538,#108,.T.);
#1945=EDGE_CURVE('',#1544,#1544,#599,.T.);
#1946=EDGE_CURVE('',#1544,#1545,#836,.T.);
#1947=EDGE_CURVE('',#1546,#1545,#109,.T.);
#1948=EDGE_CURVE('',#1547,#1546,#110,.T.);
#1949=EDGE_CURVE('',#1545,#1547,#111,.T.);
#1950=EDGE_CURVE('',#1548,#1547,#837,.T.);
#1951=EDGE_CURVE('',#1549,#1548,#838,.T.);
#1952=EDGE_CURVE('',#1550,#1549,#839,.T.);
#1953=EDGE_CURVE('',#1551,#1550,#840,.T.);
#1954=EDGE_CURVE('',#1546,#1551,#841,.T.);
#1955=EDGE_CURVE('',#1542,#1552,#842,.T.);
#1956=EDGE_CURVE('',#1553,#1552,#843,.T.);
#1957=EDGE_CURVE('',#1554,#1553,#844,.T.);
#1958=EDGE_CURVE('',#1555,#1554,#845,.T.);
#1959=EDGE_CURVE('',#1555,#1540,#846,.T.);
#1960=EDGE_CURVE('',#1556,#1556,#112,.T.);
#1961=EDGE_CURVE('',#1556,#1557,#847,.T.);
#1962=EDGE_CURVE('',#1557,#1557,#113,.T.);
#1963=EDGE_CURVE('',#1558,#1558,#600,.T.);
#1964=EDGE_CURVE('',#1558,#1559,#848,.T.);
#1965=EDGE_CURVE('',#1559,#1559,#601,.T.);
#1966=EDGE_CURVE('',#1560,#1560,#602,.T.);
#1967=EDGE_CURVE('',#1560,#1561,#849,.T.);
#1968=EDGE_CURVE('',#1561,#1561,#603,.T.);
#1969=EDGE_CURVE('',#1562,#1563,#850,.T.);
#1970=EDGE_CURVE('',#1562,#1564,#851,.T.);
#1971=EDGE_CURVE('',#1565,#1564,#852,.T.);
#1972=EDGE_CURVE('',#1563,#1565,#853,.T.);
#1973=EDGE_CURVE('',#1566,#1562,#604,.T.);
#1974=EDGE_CURVE('',#1566,#1567,#854,.T.);
#1975=EDGE_CURVE('',#1568,#1567,#605,.T.);
#1976=EDGE_CURVE('',#1564,#1568,#855,.T.);
#1977=EDGE_CURVE('',#1569,#1570,#606,.T.);
#1978=EDGE_CURVE('',#1569,#1571,#856,.T.);
#1979=EDGE_CURVE('',#1572,#1571,#607,.T.);
#1980=EDGE_CURVE('',#1570,#1572,#857,.T.);
#1981=EDGE_CURVE('',#1573,#1569,#858,.T.);
#1982=EDGE_CURVE('',#1573,#1574,#859,.T.);
#1983=EDGE_CURVE('',#1571,#1574,#860,.T.);
#1984=EDGE_CURVE('',#1575,#1575,#608,.T.);
#1985=EDGE_CURVE('',#1575,#1576,#861,.T.);
#1986=EDGE_CURVE('',#1576,#1576,#609,.T.);
#1987=EDGE_CURVE('',#1577,#1578,#862,.T.);
#1988=EDGE_CURVE('',#1577,#1579,#863,.T.);
#1989=EDGE_CURVE('',#1579,#1580,#864,.T.);
#1990=EDGE_CURVE('',#1578,#1580,#865,.T.);
#1991=EDGE_CURVE('',#1581,#1582,#866,.T.);
#1992=EDGE_CURVE('',#1583,#1581,#867,.T.);
#1993=EDGE_CURVE('',#1583,#1584,#868,.T.);
#1994=EDGE_CURVE('',#1582,#1584,#869,.T.);
#1995=EDGE_CURVE('',#1585,#1586,#870,.T.);
#1996=EDGE_CURVE('',#1586,#1587,#871,.T.);
#1997=EDGE_CURVE('',#1587,#1555,#872,.T.);
#1998=EDGE_CURVE('',#1588,#1554,#873,.T.);
#1999=EDGE_CURVE('',#1588,#1585,#874,.T.);
#2000=EDGE_CURVE('',#1589,#1590,#875,.T.);
#2001=EDGE_CURVE('',#1590,#1591,#876,.T.);
#2002=EDGE_CURVE('',#1549,#1591,#877,.T.);
#2003=EDGE_CURVE('',#1548,#1592,#878,.T.);
#2004=EDGE_CURVE('',#1592,#1589,#879,.T.);
#2005=EDGE_CURVE('',#1593,#1594,#610,.T.);
#2006=EDGE_CURVE('',#1593,#1595,#880,.T.);
#2007=EDGE_CURVE('',#1596,#1595,#611,.T.);
#2008=EDGE_CURVE('',#1597,#1596,#612,.T.);
#2009=EDGE_CURVE('',#1594,#1597,#881,.T.);
#2010=EDGE_CURVE('',#1598,#1599,#613,.T.);
#2011=EDGE_CURVE('',#1599,#1600,#882,.T.);
#2012=EDGE_CURVE('',#1601,#1600,#614,.T.);
#2013=EDGE_CURVE('',#1598,#1601,#883,.T.);
#2014=EDGE_CURVE('',#1599,#1602,#884,.T.);
#2015=EDGE_CURVE('',#1602,#1603,#885,.T.);
#2016=EDGE_CURVE('',#1600,#1603,#886,.T.);
#2017=EDGE_CURVE('',#1604,#1602,#615,.T.);
#2018=EDGE_CURVE('',#1604,#1605,#887,.T.);
#2019=EDGE_CURVE('',#1603,#1605,#616,.T.);
#2020=EDGE_CURVE('',#1606,#1573,#617,.T.);
#2021=EDGE_CURVE('',#1606,#1607,#888,.T.);
#2022=EDGE_CURVE('',#1574,#1607,#618,.T.);
#2023=EDGE_CURVE('',#1608,#1606,#889,.T.);
#2024=EDGE_CURVE('',#1608,#1609,#890,.T.);
#2025=EDGE_CURVE('',#1607,#1609,#891,.T.);
#2026=EDGE_CURVE('',#1610,#1608,#619,.T.);
#2027=EDGE_CURVE('',#1610,#1611,#892,.T.);
#2028=EDGE_CURVE('',#1609,#1611,#620,.T.);
#2029=EDGE_CURVE('',#1591,#1612,#893,.T.);
#2030=EDGE_CURVE('',#1612,#1613,#894,.T.);
#2031=EDGE_CURVE('',#1613,#1614,#895,.T.);
#2032=EDGE_CURVE('',#1615,#1614,#896,.T.);
#2033=EDGE_CURVE('',#1596,#1615,#897,.T.);
#2034=EDGE_CURVE('',#1611,#1596,#898,.T.);
#2035=EDGE_CURVE('',#1570,#1610,#899,.T.);
#2036=EDGE_CURVE('',#1564,#1572,#900,.T.);
#2037=EDGE_CURVE('',#1578,#1568,#901,.T.);
#2038=EDGE_CURVE('',#1580,#1591,#902,.T.);
#2039=EDGE_CURVE('',#1616,#1615,#621,.T.);
#2040=EDGE_CURVE('',#1597,#1616,#903,.T.);
#2041=EDGE_CURVE('',#1582,#1617,#904,.T.);
#2042=EDGE_CURVE('',#1617,#1618,#905,.T.);
#2043=EDGE_CURVE('',#1618,#1616,#906,.T.);
#2044=EDGE_CURVE('',#1614,#1619,#907,.T.);
#2045=EDGE_CURVE('',#1619,#1577,#908,.T.);
#2046=EDGE_CURVE('',#1567,#1581,#909,.T.);
#2047=EDGE_CURVE('',#1613,#1620,#910,.T.);
#2048=EDGE_CURVE('',#1619,#1620,#911,.T.);
#2049=EDGE_CURVE('',#1620,#1579,#912,.T.);
#2050=EDGE_CURVE('',#1617,#1621,#913,.T.);
#2051=EDGE_CURVE('',#1621,#1622,#914,.T.);
#2052=EDGE_CURVE('',#1618,#1622,#915,.T.);
#2053=EDGE_CURVE('',#1623,#1624,#916,.T.);
#2054=EDGE_CURVE('',#1624,#1625,#917,.T.);
#2055=EDGE_CURVE('',#1553,#1625,#918,.T.);
#2056=EDGE_CURVE('',#1552,#1626,#919,.T.);
#2057=EDGE_CURVE('',#1626,#1623,#920,.T.);
#2058=EDGE_CURVE('',#1612,#1550,#921,.T.);
#2059=EDGE_CURVE('',#1627,#1628,#922,.T.);
#2060=EDGE_CURVE('',#1628,#1629,#923,.T.);
#2061=EDGE_CURVE('',#1629,#1551,#924,.T.);
#2062=EDGE_CURVE('',#1612,#1627,#925,.T.);
#2063=EDGE_CURVE('',#1589,#1628,#926,.T.);
#2064=EDGE_CURVE('',#1627,#1590,#927,.T.);
#2065=EDGE_CURVE('',#1592,#1629,#928,.T.);
#2066=EDGE_CURVE('',#1605,#1565,#622,.T.);
#2067=EDGE_CURVE('',#1563,#1604,#623,.T.);
#2068=EDGE_CURVE('',#1566,#1594,#929,.T.);
#2069=EDGE_CURVE('',#1622,#1625,#930,.T.);
#2070=EDGE_CURVE('',#1625,#1588,#931,.T.);
#2071=EDGE_CURVE('',#1588,#1583,#932,.T.);
#2072=EDGE_CURVE('',#1585,#1624,#933,.T.);
#2073=EDGE_CURVE('',#1623,#1586,#934,.T.);
#2074=EDGE_CURVE('',#1587,#1626,#935,.T.);
#2075=EDGE_CURVE('',#1584,#1621,#936,.T.);
#2076=EDGE_CURVE('',#1630,#1631,#937,.T.);
#2077=EDGE_CURVE('',#1632,#1630,#938,.T.);
#2078=EDGE_CURVE('',#1633,#1632,#939,.T.);
#2079=EDGE_CURVE('',#1634,#1633,#940,.T.);
#2080=EDGE_CURVE('',#1635,#1634,#941,.T.);
#2081=EDGE_CURVE('',#1631,#1635,#942,.T.);
#2082=EDGE_CURVE('',#1636,#1637,#943,.T.);
#2083=EDGE_CURVE('',#1638,#1636,#944,.T.);
#2084=EDGE_CURVE('',#1639,#1638,#945,.T.);
#2085=EDGE_CURVE('',#1640,#1639,#946,.T.);
#2086=EDGE_CURVE('',#1641,#1640,#947,.T.);
#2087=EDGE_CURVE('',#1641,#1637,#948,.T.);
#2088=EDGE_CURVE('',#1642,#1636,#949,.T.);
#2089=EDGE_CURVE('',#1643,#1642,#950,.T.);
#2090=EDGE_CURVE('',#1644,#1643,#951,.T.);
#2091=EDGE_CURVE('',#1644,#1638,#952,.T.);
#2092=EDGE_CURVE('',#1645,#1645,#624,.T.);
#2093=EDGE_CURVE('',#1645,#1646,#953,.T.);
#2094=EDGE_CURVE('',#1646,#1646,#625,.T.);
#2095=EDGE_CURVE('',#1647,#1635,#954,.T.);
#2096=EDGE_CURVE('',#1647,#1648,#955,.T.);
#2097=EDGE_CURVE('',#1649,#1648,#956,.T.);
#2098=EDGE_CURVE('',#1649,#1650,#957,.T.);
#2099=EDGE_CURVE('',#1631,#1650,#958,.T.);
#2100=EDGE_CURVE('',#1651,#1652,#959,.T.);
#2101=EDGE_CURVE('',#1651,#1653,#960,.T.);
#2102=EDGE_CURVE('',#1654,#1653,#961,.T.);
#2103=EDGE_CURVE('',#1652,#1654,#962,.T.);
#2104=EDGE_CURVE('',#1652,#1647,#626,.T.);
#2105=EDGE_CURVE('',#1648,#1654,#627,.T.);
#2106=EDGE_CURVE('',#1644,#1655,#628,.T.);
#2107=EDGE_CURVE('',#1650,#1642,#629,.T.);
#2108=EDGE_CURVE('',#1655,#1649,#963,.T.);
#2109=EDGE_CURVE('',#1656,#1655,#964,.T.);
#2110=EDGE_CURVE('',#1657,#1649,#965,.T.);
#2111=EDGE_CURVE('',#1656,#1657,#966,.T.);
#2112=EDGE_CURVE('',#1658,#1639,#967,.T.);
#2113=EDGE_CURVE('',#1658,#1659,#968,.T.);
#2114=EDGE_CURVE('',#1640,#1659,#969,.T.);
#2115=EDGE_CURVE('',#1659,#1660,#970,.T.);
#2116=EDGE_CURVE('',#1641,#1660,#971,.T.);
#2117=EDGE_CURVE('',#1661,#1632,#972,.T.);
#2118=EDGE_CURVE('',#1661,#1662,#973,.T.);
#2119=EDGE_CURVE('',#1662,#1633,#974,.T.);
#2120=EDGE_CURVE('',#1662,#1663,#975,.T.);
#2121=EDGE_CURVE('',#1634,#1663,#976,.T.);
#2122=EDGE_CURVE('',#1598,#1664,#977,.T.);
#2123=EDGE_CURVE('',#1664,#1665,#630,.T.);
#2124=EDGE_CURVE('',#1666,#1665,#978,.T.);
#2125=EDGE_CURVE('',#1666,#1658,#979,.T.);
#2126=EDGE_CURVE('',#1656,#1667,#631,.T.);
#2127=EDGE_CURVE('',#1667,#1668,#980,.T.);
#2128=EDGE_CURVE('',#1668,#1669,#632,.T.);
#2129=EDGE_CURVE('',#1670,#1669,#981,.T.);
#2130=EDGE_CURVE('',#1671,#1670,#633,.T.);
#2131=EDGE_CURVE('',#1593,#1671,#982,.T.);
#2132=EDGE_CURVE('',#1663,#1672,#983,.T.);
#2133=EDGE_CURVE('',#1672,#1673,#984,.T.);
#2134=EDGE_CURVE('',#1673,#1674,#634,.T.);
#2135=EDGE_CURVE('',#1674,#1675,#985,.T.);
#2136=EDGE_CURVE('',#1675,#1651,#635,.T.);
#2137=EDGE_CURVE('',#1676,#1630,#986,.T.);
#2138=EDGE_CURVE('',#1661,#1676,#987,.T.);
#2139=EDGE_CURVE('',#1637,#1677,#988,.T.);
#2140=EDGE_CURVE('',#1677,#1678,#989,.T.);
#2141=EDGE_CURVE('',#1678,#1679,#990,.T.);
#2142=EDGE_CURVE('',#1679,#1680,#636,.T.);
#2143=EDGE_CURVE('',#1680,#1681,#991,.T.);
#2144=EDGE_CURVE('',#1681,#1676,#992,.T.);
#2145=EDGE_CURVE('',#1682,#1601,#993,.T.);
#2146=EDGE_CURVE('',#1664,#1682,#994,.T.);
#2147=EDGE_CURVE('',#1683,#1657,#637,.T.);
#2148=EDGE_CURVE('',#1667,#1683,#995,.T.);
#2149=EDGE_CURVE('',#1595,#1684,#996,.T.);
#2150=EDGE_CURVE('',#1684,#1685,#638,.T.);
#2151=EDGE_CURVE('',#1685,#1686,#997,.T.);
#2152=EDGE_CURVE('',#1686,#1687,#639,.T.);
#2153=EDGE_CURVE('',#1687,#1683,#998,.T.);
#2154=EDGE_CURVE('',#1653,#1688,#640,.T.);
#2155=EDGE_CURVE('',#1688,#1689,#999,.T.);
#2156=EDGE_CURVE('',#1689,#1690,#641,.T.);
#2157=EDGE_CURVE('',#1690,#1691,#1000,.T.);
#2158=EDGE_CURVE('',#1691,#1682,#642,.T.);
#2159=EDGE_CURVE('',#1672,#1681,#1001,.T.);
#2160=EDGE_CURVE('',#1660,#1677,#1002,.T.);
#2161=EDGE_CURVE('',#1678,#1666,#1003,.T.);
#2162=EDGE_CURVE('',#1691,#1680,#1004,.T.);
#2163=EDGE_CURVE('',#1673,#1690,#1005,.T.);
#2164=EDGE_CURVE('',#1674,#1689,#1006,.T.);
#2165=EDGE_CURVE('',#1675,#1688,#1007,.T.);
#2166=EDGE_CURVE('',#1668,#1687,#1008,.T.);
#2167=EDGE_CURVE('',#1669,#1686,#1009,.T.);
#2168=EDGE_CURVE('',#1670,#1685,#1010,.T.);
#2169=EDGE_CURVE('',#1684,#1671,#1011,.T.);
#2170=EDGE_CURVE('',#1665,#1692,#1012,.T.);
#2171=EDGE_CURVE('',#1692,#1679,#1013,.T.);
#2172=EDGE_CURVE('',#1693,#1693,#643,.T.);
#2173=EDGE_CURVE('',#1694,#1694,#644,.T.);
#2174=EDGE_CURVE('',#1694,#1693,#1014,.T.);
#2175=EDGE_CURVE('',#1695,#1695,#645,.T.);
#2176=EDGE_CURVE('',#1695,#1696,#1015,.T.);
#2177=EDGE_CURVE('',#1696,#1696,#646,.T.);
#2178=EDGE_CURVE('',#1697,#1697,#647,.T.);
#2179=EDGE_CURVE('',#1697,#1698,#1016,.T.);
#2180=EDGE_CURVE('',#1698,#1698,#648,.T.);
#2181=EDGE_CURVE('',#1699,#1699,#649,.T.);
#2182=EDGE_CURVE('',#1699,#1700,#1017,.T.);
#2183=EDGE_CURVE('',#1700,#1700,#650,.T.);
#2184=EDGE_CURVE('',#1701,#1701,#651,.T.);
#2185=EDGE_CURVE('',#1702,#1702,#652,.T.);
#2186=EDGE_CURVE('',#1702,#1701,#1018,.T.);
#2187=EDGE_CURVE('',#1703,#1703,#653,.T.);
#2188=EDGE_CURVE('',#1703,#1704,#1019,.T.);
#2189=EDGE_CURVE('',#1704,#1704,#654,.T.);
#2190=ORIENTED_EDGE('',*,*,#1705,.F.);
#2191=ORIENTED_EDGE('',*,*,#1706,.F.);
#2192=ORIENTED_EDGE('',*,*,#1707,.F.);
#2193=ORIENTED_EDGE('',*,*,#1708,.T.);
#2194=ORIENTED_EDGE('',*,*,#1709,.F.);
#2195=ORIENTED_EDGE('',*,*,#1706,.T.);
#2196=ORIENTED_EDGE('',*,*,#1710,.F.);
#2197=ORIENTED_EDGE('',*,*,#1708,.F.);
#2198=ORIENTED_EDGE('',*,*,#1711,.F.);
#2199=ORIENTED_EDGE('',*,*,#1712,.T.);
#2200=ORIENTED_EDGE('',*,*,#1713,.F.);
#2201=ORIENTED_EDGE('',*,*,#1712,.F.);
#2202=ORIENTED_EDGE('',*,*,#1714,.F.);
#2203=ORIENTED_EDGE('',*,*,#1715,.F.);
#2204=ORIENTED_EDGE('',*,*,#1716,.F.);
#2205=ORIENTED_EDGE('',*,*,#1717,.T.);
#2206=ORIENTED_EDGE('',*,*,#1718,.F.);
#2207=ORIENTED_EDGE('',*,*,#1717,.F.);
#2208=ORIENTED_EDGE('',*,*,#1714,.T.);
#2209=ORIENTED_EDGE('',*,*,#1716,.T.);
#2210=ORIENTED_EDGE('',*,*,#1719,.T.);
#2211=ORIENTED_EDGE('',*,*,#1720,.T.);
#2212=ORIENTED_EDGE('',*,*,#1721,.F.);
#2213=ORIENTED_EDGE('',*,*,#1722,.F.);
#2214=ORIENTED_EDGE('',*,*,#1723,.T.);
#2215=ORIENTED_EDGE('',*,*,#1724,.F.);
#2216=ORIENTED_EDGE('',*,*,#1725,.T.);
#2217=ORIENTED_EDGE('',*,*,#1726,.T.);
#2218=ORIENTED_EDGE('',*,*,#1725,.F.);
#2219=ORIENTED_EDGE('',*,*,#1726,.F.);
#2220=ORIENTED_EDGE('',*,*,#1727,.F.);
#2221=ORIENTED_EDGE('',*,*,#1728,.T.);
#2222=ORIENTED_EDGE('',*,*,#1729,.T.);
#2223=ORIENTED_EDGE('',*,*,#1728,.F.);
#2224=ORIENTED_EDGE('',*,*,#1729,.F.);
#2225=ORIENTED_EDGE('',*,*,#1730,.F.);
#2226=ORIENTED_EDGE('',*,*,#1720,.F.);
#2227=ORIENTED_EDGE('',*,*,#1731,.F.);
#2228=ORIENTED_EDGE('',*,*,#1732,.F.);
#2229=ORIENTED_EDGE('',*,*,#1733,.F.);
#2230=ORIENTED_EDGE('',*,*,#1734,.F.);
#2231=ORIENTED_EDGE('',*,*,#1735,.F.);
#2232=ORIENTED_EDGE('',*,*,#1736,.F.);
#2233=ORIENTED_EDGE('',*,*,#1737,.F.);
#2234=ORIENTED_EDGE('',*,*,#1738,.F.);
#2235=ORIENTED_EDGE('',*,*,#1739,.F.);
#2236=ORIENTED_EDGE('',*,*,#1740,.T.);
#2237=ORIENTED_EDGE('',*,*,#1736,.T.);
#2238=ORIENTED_EDGE('',*,*,#1741,.F.);
#2239=ORIENTED_EDGE('',*,*,#1742,.F.);
#2240=ORIENTED_EDGE('',*,*,#1743,.F.);
#2241=ORIENTED_EDGE('',*,*,#1744,.T.);
#2242=ORIENTED_EDGE('',*,*,#1745,.T.);
#2243=ORIENTED_EDGE('',*,*,#1745,.F.);
#2244=ORIENTED_EDGE('',*,*,#1746,.T.);
#2245=ORIENTED_EDGE('',*,*,#1747,.F.);
#2246=ORIENTED_EDGE('',*,*,#1746,.F.);
#2247=ORIENTED_EDGE('',*,*,#1734,.T.);
#2248=ORIENTED_EDGE('',*,*,#1748,.F.);
#2249=ORIENTED_EDGE('',*,*,#1749,.T.);
#2250=ORIENTED_EDGE('',*,*,#1750,.F.);
#2251=ORIENTED_EDGE('',*,*,#1751,.T.);
#2252=ORIENTED_EDGE('',*,*,#1752,.F.);
#2253=ORIENTED_EDGE('',*,*,#1753,.F.);
#2254=ORIENTED_EDGE('',*,*,#1754,.T.);
#2255=ORIENTED_EDGE('',*,*,#1755,.F.);
#2256=ORIENTED_EDGE('',*,*,#1756,.F.);
#2257=ORIENTED_EDGE('',*,*,#1757,.F.);
#2258=ORIENTED_EDGE('',*,*,#1756,.T.);
#2259=ORIENTED_EDGE('',*,*,#1758,.F.);
#2260=ORIENTED_EDGE('',*,*,#1749,.F.);
#2261=ORIENTED_EDGE('',*,*,#1759,.F.);
#2262=ORIENTED_EDGE('',*,*,#1743,.T.);
#2263=ORIENTED_EDGE('',*,*,#1742,.T.);
#2264=ORIENTED_EDGE('',*,*,#1760,.F.);
#2265=ORIENTED_EDGE('',*,*,#1751,.F.);
#2266=ORIENTED_EDGE('',*,*,#1761,.F.);
#2267=ORIENTED_EDGE('',*,*,#1762,.T.);
#2268=ORIENTED_EDGE('',*,*,#1761,.T.);
#2269=ORIENTED_EDGE('',*,*,#1763,.F.);
#2270=ORIENTED_EDGE('',*,*,#1764,.F.);
#2271=ORIENTED_EDGE('',*,*,#1765,.F.);
#2272=ORIENTED_EDGE('',*,*,#1766,.T.);
#2273=ORIENTED_EDGE('',*,*,#1767,.T.);
#2274=ORIENTED_EDGE('',*,*,#1738,.T.);
#2275=ORIENTED_EDGE('',*,*,#1767,.F.);
#2276=ORIENTED_EDGE('',*,*,#1768,.T.);
#2277=ORIENTED_EDGE('',*,*,#1769,.F.);
#2278=ORIENTED_EDGE('',*,*,#1739,.T.);
#2279=ORIENTED_EDGE('',*,*,#1715,.T.);
#2280=ORIENTED_EDGE('',*,*,#1723,.F.);
#2281=ORIENTED_EDGE('',*,*,#1770,.T.);
#2282=ORIENTED_EDGE('',*,*,#1771,.T.);
#2283=ORIENTED_EDGE('',*,*,#1731,.T.);
#2284=ORIENTED_EDGE('',*,*,#1719,.F.);
#2285=ORIENTED_EDGE('',*,*,#1771,.F.);
#2286=ORIENTED_EDGE('',*,*,#1772,.T.);
#2287=ORIENTED_EDGE('',*,*,#1773,.F.);
#2288=ORIENTED_EDGE('',*,*,#1732,.T.);
#2289=ORIENTED_EDGE('',*,*,#1774,.T.);
#2290=ORIENTED_EDGE('',*,*,#1775,.T.);
#2291=ORIENTED_EDGE('',*,*,#1776,.T.);
#2292=ORIENTED_EDGE('',*,*,#1777,.T.);
#2293=ORIENTED_EDGE('',*,*,#1778,.T.);
#2294=ORIENTED_EDGE('',*,*,#1779,.T.);
#2295=ORIENTED_EDGE('',*,*,#1721,.T.);
#2296=ORIENTED_EDGE('',*,*,#1730,.T.);
#2297=ORIENTED_EDGE('',*,*,#1752,.T.);
#2298=ORIENTED_EDGE('',*,*,#1760,.T.);
#2299=ORIENTED_EDGE('',*,*,#1741,.T.);
#2300=ORIENTED_EDGE('',*,*,#1735,.T.);
#2301=ORIENTED_EDGE('',*,*,#1747,.T.);
#2302=ORIENTED_EDGE('',*,*,#1727,.T.);
#2303=ORIENTED_EDGE('',*,*,#1780,.F.);
#2304=ORIENTED_EDGE('',*,*,#1781,.F.);
#2305=ORIENTED_EDGE('',*,*,#1782,.F.);
#2306=ORIENTED_EDGE('',*,*,#1764,.T.);
#2307=ORIENTED_EDGE('',*,*,#1779,.F.);
#2308=ORIENTED_EDGE('',*,*,#1783,.F.);
#2309=ORIENTED_EDGE('',*,*,#1784,.F.);
#2310=ORIENTED_EDGE('',*,*,#1772,.F.);
#2311=ORIENTED_EDGE('',*,*,#1770,.F.);
#2312=ORIENTED_EDGE('',*,*,#1722,.T.);
#2313=ORIENTED_EDGE('',*,*,#1769,.T.);
#2314=ORIENTED_EDGE('',*,*,#1785,.T.);
#2315=ORIENTED_EDGE('',*,*,#1774,.F.);
#2316=ORIENTED_EDGE('',*,*,#1740,.F.);
#2317=ORIENTED_EDGE('',*,*,#1718,.T.);
#2318=ORIENTED_EDGE('',*,*,#1775,.F.);
#2319=ORIENTED_EDGE('',*,*,#1785,.F.);
#2320=ORIENTED_EDGE('',*,*,#1768,.F.);
#2321=ORIENTED_EDGE('',*,*,#1766,.F.);
#2322=ORIENTED_EDGE('',*,*,#1786,.F.);
#2323=ORIENTED_EDGE('',*,*,#1787,.F.);
#2324=ORIENTED_EDGE('',*,*,#1783,.T.);
#2325=ORIENTED_EDGE('',*,*,#1778,.F.);
#2326=ORIENTED_EDGE('',*,*,#1788,.F.);
#2327=ORIENTED_EDGE('',*,*,#1789,.F.);
#2328=ORIENTED_EDGE('',*,*,#1790,.F.);
#2329=ORIENTED_EDGE('',*,*,#1791,.F.);
#2330=ORIENTED_EDGE('',*,*,#1792,.F.);
#2331=ORIENTED_EDGE('',*,*,#1790,.T.);
#2332=ORIENTED_EDGE('',*,*,#1793,.F.);
#2333=ORIENTED_EDGE('',*,*,#1794,.F.);
#2334=ORIENTED_EDGE('',*,*,#1795,.F.);
#2335=ORIENTED_EDGE('',*,*,#1794,.T.);
#2336=ORIENTED_EDGE('',*,*,#1796,.F.);
#2337=ORIENTED_EDGE('',*,*,#1797,.F.);
#2338=ORIENTED_EDGE('',*,*,#1798,.F.);
#2339=ORIENTED_EDGE('',*,*,#1797,.T.);
#2340=ORIENTED_EDGE('',*,*,#1799,.F.);
#2341=ORIENTED_EDGE('',*,*,#1754,.F.);
#2342=ORIENTED_EDGE('',*,*,#1800,.F.);
#2343=ORIENTED_EDGE('',*,*,#1781,.T.);
#2344=ORIENTED_EDGE('',*,*,#1801,.F.);
#2345=ORIENTED_EDGE('',*,*,#1802,.F.);
#2346=ORIENTED_EDGE('',*,*,#1803,.F.);
#2347=ORIENTED_EDGE('',*,*,#1802,.T.);
#2348=ORIENTED_EDGE('',*,*,#1804,.F.);
#2349=ORIENTED_EDGE('',*,*,#1805,.F.);
#2350=ORIENTED_EDGE('',*,*,#1806,.T.);
#2351=ORIENTED_EDGE('',*,*,#1805,.T.);
#2352=ORIENTED_EDGE('',*,*,#1807,.F.);
#2353=ORIENTED_EDGE('',*,*,#1808,.F.);
#2354=ORIENTED_EDGE('',*,*,#1809,.T.);
#2355=ORIENTED_EDGE('',*,*,#1808,.T.);
#2356=ORIENTED_EDGE('',*,*,#1810,.F.);
#2357=ORIENTED_EDGE('',*,*,#1811,.T.);
#2358=ORIENTED_EDGE('',*,*,#1787,.T.);
#2359=ORIENTED_EDGE('',*,*,#1812,.T.);
#2360=ORIENTED_EDGE('',*,*,#1813,.T.);
#2361=ORIENTED_EDGE('',*,*,#1814,.T.);
#2362=ORIENTED_EDGE('',*,*,#1776,.F.);
#2363=ORIENTED_EDGE('',*,*,#1815,.F.);
#2364=ORIENTED_EDGE('',*,*,#1816,.T.);
#2365=ORIENTED_EDGE('',*,*,#1817,.F.);
#2366=ORIENTED_EDGE('',*,*,#1788,.T.);
#2367=ORIENTED_EDGE('',*,*,#1777,.F.);
#2368=ORIENTED_EDGE('',*,*,#1814,.F.);
#2369=ORIENTED_EDGE('',*,*,#1813,.F.);
#2370=ORIENTED_EDGE('',*,*,#1818,.F.);
#2371=ORIENTED_EDGE('',*,*,#1819,.T.);
#2372=ORIENTED_EDGE('',*,*,#1820,.F.);
#2373=ORIENTED_EDGE('',*,*,#1821,.F.);
#2374=ORIENTED_EDGE('',*,*,#1822,.F.);
#2375=ORIENTED_EDGE('',*,*,#1823,.F.);
#2376=ORIENTED_EDGE('',*,*,#1824,.T.);
#2377=ORIENTED_EDGE('',*,*,#1825,.F.);
#2378=ORIENTED_EDGE('',*,*,#1816,.F.);
#2379=ORIENTED_EDGE('',*,*,#1826,.T.);
#2380=ORIENTED_EDGE('',*,*,#1827,.T.);
#2381=ORIENTED_EDGE('',*,*,#1828,.F.);
#2382=ORIENTED_EDGE('',*,*,#1824,.F.);
#2383=ORIENTED_EDGE('',*,*,#1829,.T.);
#2384=ORIENTED_EDGE('',*,*,#1830,.T.);
#2385=ORIENTED_EDGE('',*,*,#1831,.F.);
#2386=ORIENTED_EDGE('',*,*,#1827,.F.);
#2387=ORIENTED_EDGE('',*,*,#1832,.F.);
#2388=ORIENTED_EDGE('',*,*,#1833,.T.);
#2389=ORIENTED_EDGE('',*,*,#1834,.F.);
#2390=ORIENTED_EDGE('',*,*,#1830,.F.);
#2391=ORIENTED_EDGE('',*,*,#1835,.F.);
#2392=ORIENTED_EDGE('',*,*,#1836,.T.);
#2393=ORIENTED_EDGE('',*,*,#1837,.F.);
#2394=ORIENTED_EDGE('',*,*,#1838,.F.);
#2395=ORIENTED_EDGE('',*,*,#1839,.F.);
#2396=ORIENTED_EDGE('',*,*,#1840,.T.);
#2397=ORIENTED_EDGE('',*,*,#1841,.F.);
#2398=ORIENTED_EDGE('',*,*,#1836,.F.);
#2399=ORIENTED_EDGE('',*,*,#1821,.T.);
#2400=ORIENTED_EDGE('',*,*,#1842,.T.);
#2401=ORIENTED_EDGE('',*,*,#1843,.F.);
#2402=ORIENTED_EDGE('',*,*,#1844,.F.);
#2403=ORIENTED_EDGE('',*,*,#1845,.F.);
#2404=ORIENTED_EDGE('',*,*,#1846,.F.);
#2405=ORIENTED_EDGE('',*,*,#1847,.T.);
#2406=ORIENTED_EDGE('',*,*,#1848,.F.);
#2407=ORIENTED_EDGE('',*,*,#1849,.F.);
#2408=ORIENTED_EDGE('',*,*,#1850,.T.);
#2409=ORIENTED_EDGE('',*,*,#1851,.T.);
#2410=ORIENTED_EDGE('',*,*,#1852,.F.);
#2411=ORIENTED_EDGE('',*,*,#1853,.T.);
#2412=ORIENTED_EDGE('',*,*,#1854,.T.);
#2413=ORIENTED_EDGE('',*,*,#1855,.F.);
#2414=ORIENTED_EDGE('',*,*,#1856,.T.);
#2415=ORIENTED_EDGE('',*,*,#1857,.T.);
#2416=ORIENTED_EDGE('',*,*,#1858,.T.);
#2417=ORIENTED_EDGE('',*,*,#1859,.T.);
#2418=ORIENTED_EDGE('',*,*,#1860,.T.);
#2419=ORIENTED_EDGE('',*,*,#1861,.T.);
#2420=ORIENTED_EDGE('',*,*,#1862,.T.);
#2421=ORIENTED_EDGE('',*,*,#1863,.F.);
#2422=ORIENTED_EDGE('',*,*,#1864,.T.);
#2423=ORIENTED_EDGE('',*,*,#1865,.F.);
#2424=ORIENTED_EDGE('',*,*,#1819,.F.);
#2425=ORIENTED_EDGE('',*,*,#1866,.T.);
#2426=ORIENTED_EDGE('',*,*,#1811,.F.);
#2427=ORIENTED_EDGE('',*,*,#1867,.F.);
#2428=ORIENTED_EDGE('',*,*,#1868,.T.);
#2429=ORIENTED_EDGE('',*,*,#1869,.F.);
#2430=ORIENTED_EDGE('',*,*,#1833,.F.);
#2431=ORIENTED_EDGE('',*,*,#1870,.F.);
#2432=ORIENTED_EDGE('',*,*,#1871,.T.);
#2433=ORIENTED_EDGE('',*,*,#1872,.F.);
#2434=ORIENTED_EDGE('',*,*,#1868,.F.);
#2435=ORIENTED_EDGE('',*,*,#1873,.F.);
#2436=ORIENTED_EDGE('',*,*,#1874,.T.);
#2437=ORIENTED_EDGE('',*,*,#1875,.F.);
#2438=ORIENTED_EDGE('',*,*,#1876,.F.);
#2439=ORIENTED_EDGE('',*,*,#1871,.F.);
#2440=ORIENTED_EDGE('',*,*,#1877,.T.);
#2441=ORIENTED_EDGE('',*,*,#1878,.T.);
#2442=ORIENTED_EDGE('',*,*,#1879,.T.);
#2443=ORIENTED_EDGE('',*,*,#1880,.F.);
#2444=ORIENTED_EDGE('',*,*,#1874,.F.);
#2445=ORIENTED_EDGE('',*,*,#1881,.T.);
#2446=ORIENTED_EDGE('',*,*,#1822,.T.);
#2447=ORIENTED_EDGE('',*,*,#1844,.T.);
#2448=ORIENTED_EDGE('',*,*,#1882,.F.);
#2449=ORIENTED_EDGE('',*,*,#1852,.T.);
#2450=ORIENTED_EDGE('',*,*,#1883,.T.);
#2451=ORIENTED_EDGE('',*,*,#1884,.F.);
#2452=ORIENTED_EDGE('',*,*,#1885,.T.);
#2453=ORIENTED_EDGE('',*,*,#1886,.F.);
#2454=ORIENTED_EDGE('',*,*,#1887,.F.);
#2455=ORIENTED_EDGE('',*,*,#1888,.F.);
#2456=ORIENTED_EDGE('',*,*,#1889,.T.);
#2457=ORIENTED_EDGE('',*,*,#1890,.F.);
#2458=ORIENTED_EDGE('',*,*,#1885,.F.);
#2459=ORIENTED_EDGE('',*,*,#1869,.T.);
#2460=ORIENTED_EDGE('',*,*,#1872,.T.);
#2461=ORIENTED_EDGE('',*,*,#1891,.T.);
#2462=ORIENTED_EDGE('',*,*,#1886,.T.);
#2463=ORIENTED_EDGE('',*,*,#1890,.T.);
#2464=ORIENTED_EDGE('',*,*,#1892,.T.);
#2465=ORIENTED_EDGE('',*,*,#1837,.T.);
#2466=ORIENTED_EDGE('',*,*,#1841,.T.);
#2467=ORIENTED_EDGE('',*,*,#1893,.T.);
#2468=ORIENTED_EDGE('',*,*,#1820,.T.);
#2469=ORIENTED_EDGE('',*,*,#1865,.T.);
#2470=ORIENTED_EDGE('',*,*,#1810,.T.);
#2471=ORIENTED_EDGE('',*,*,#1807,.T.);
#2472=ORIENTED_EDGE('',*,*,#1804,.T.);
#2473=ORIENTED_EDGE('',*,*,#1801,.T.);
#2474=ORIENTED_EDGE('',*,*,#1780,.T.);
#2475=ORIENTED_EDGE('',*,*,#1763,.T.);
#2476=ORIENTED_EDGE('',*,*,#1750,.T.);
#2477=ORIENTED_EDGE('',*,*,#1758,.T.);
#2478=ORIENTED_EDGE('',*,*,#1755,.T.);
#2479=ORIENTED_EDGE('',*,*,#1799,.T.);
#2480=ORIENTED_EDGE('',*,*,#1796,.T.);
#2481=ORIENTED_EDGE('',*,*,#1793,.T.);
#2482=ORIENTED_EDGE('',*,*,#1789,.T.);
#2483=ORIENTED_EDGE('',*,*,#1817,.T.);
#2484=ORIENTED_EDGE('',*,*,#1825,.T.);
#2485=ORIENTED_EDGE('',*,*,#1828,.T.);
#2486=ORIENTED_EDGE('',*,*,#1831,.T.);
#2487=ORIENTED_EDGE('',*,*,#1834,.T.);
#2488=ORIENTED_EDGE('',*,*,#1894,.F.);
#2489=ORIENTED_EDGE('',*,*,#1895,.T.);
#2490=ORIENTED_EDGE('',*,*,#1896,.F.);
#2491=ORIENTED_EDGE('',*,*,#1895,.F.);
#2492=ORIENTED_EDGE('',*,*,#1894,.T.);
#2493=ORIENTED_EDGE('',*,*,#1897,.F.);
#2494=ORIENTED_EDGE('',*,*,#1898,.T.);
#2495=ORIENTED_EDGE('',*,*,#1899,.T.);
#2496=ORIENTED_EDGE('',*,*,#1900,.F.);
#2497=ORIENTED_EDGE('',*,*,#1901,.F.);
#2498=ORIENTED_EDGE('',*,*,#1902,.F.);
#2499=ORIENTED_EDGE('',*,*,#1878,.F.);
#2500=ORIENTED_EDGE('',*,*,#1903,.T.);
#2501=ORIENTED_EDGE('',*,*,#1904,.T.);
#2502=ORIENTED_EDGE('',*,*,#1855,.T.);
#2503=ORIENTED_EDGE('',*,*,#1883,.F.);
#2504=ORIENTED_EDGE('',*,*,#1851,.F.);
#2505=ORIENTED_EDGE('',*,*,#1905,.F.);
#2506=ORIENTED_EDGE('',*,*,#1879,.F.);
#2507=ORIENTED_EDGE('',*,*,#1902,.T.);
#2508=ORIENTED_EDGE('',*,*,#1906,.F.);
#2509=ORIENTED_EDGE('',*,*,#1907,.F.);
#2510=ORIENTED_EDGE('',*,*,#1906,.T.);
#2511=ORIENTED_EDGE('',*,*,#1901,.T.);
#2512=ORIENTED_EDGE('',*,*,#1850,.F.);
#2513=ORIENTED_EDGE('',*,*,#1908,.T.);
#2514=ORIENTED_EDGE('',*,*,#1909,.F.);
#2515=ORIENTED_EDGE('',*,*,#1910,.T.);
#2516=ORIENTED_EDGE('',*,*,#1853,.F.);
#2517=ORIENTED_EDGE('',*,*,#1910,.F.);
#2518=ORIENTED_EDGE('',*,*,#1911,.F.);
#2519=ORIENTED_EDGE('',*,*,#1877,.F.);
#2520=ORIENTED_EDGE('',*,*,#1854,.F.);
#2521=ORIENTED_EDGE('',*,*,#1711,.T.);
#2522=ORIENTED_EDGE('',*,*,#1904,.F.);
#2523=ORIENTED_EDGE('',*,*,#1912,.F.);
#2524=ORIENTED_EDGE('',*,*,#1913,.T.);
#2525=ORIENTED_EDGE('',*,*,#1856,.F.);
#2526=ORIENTED_EDGE('',*,*,#1713,.T.);
#2527=ORIENTED_EDGE('',*,*,#1913,.F.);
#2528=ORIENTED_EDGE('',*,*,#1914,.F.);
#2529=ORIENTED_EDGE('',*,*,#1915,.T.);
#2530=ORIENTED_EDGE('',*,*,#1857,.F.);
#2531=ORIENTED_EDGE('',*,*,#1915,.F.);
#2532=ORIENTED_EDGE('',*,*,#1916,.F.);
#2533=ORIENTED_EDGE('',*,*,#1908,.F.);
#2534=ORIENTED_EDGE('',*,*,#1858,.F.);
#2535=ORIENTED_EDGE('',*,*,#1909,.T.);
#2536=ORIENTED_EDGE('',*,*,#1916,.T.);
#2537=ORIENTED_EDGE('',*,*,#1914,.T.);
#2538=ORIENTED_EDGE('',*,*,#1912,.T.);
#2539=ORIENTED_EDGE('',*,*,#1903,.F.);
#2540=ORIENTED_EDGE('',*,*,#1911,.T.);
#2541=ORIENTED_EDGE('',*,*,#1917,.T.);
#2542=ORIENTED_EDGE('',*,*,#1918,.T.);
#2543=ORIENTED_EDGE('',*,*,#1919,.F.);
#2544=ORIENTED_EDGE('',*,*,#1920,.T.);
#2545=ORIENTED_EDGE('',*,*,#1921,.T.);
#2546=ORIENTED_EDGE('',*,*,#1922,.T.);
#2547=ORIENTED_EDGE('',*,*,#1765,.T.);
#2548=ORIENTED_EDGE('',*,*,#1737,.T.);
#2549=ORIENTED_EDGE('',*,*,#1744,.F.);
#2550=ORIENTED_EDGE('',*,*,#1759,.T.);
#2551=ORIENTED_EDGE('',*,*,#1762,.F.);
#2552=ORIENTED_EDGE('',*,*,#1782,.T.);
#2553=ORIENTED_EDGE('',*,*,#1800,.T.);
#2554=ORIENTED_EDGE('',*,*,#1803,.T.);
#2555=ORIENTED_EDGE('',*,*,#1806,.F.);
#2556=ORIENTED_EDGE('',*,*,#1809,.F.);
#2557=ORIENTED_EDGE('',*,*,#1866,.F.);
#2558=ORIENTED_EDGE('',*,*,#1818,.T.);
#2559=ORIENTED_EDGE('',*,*,#1881,.F.);
#2560=ORIENTED_EDGE('',*,*,#1873,.T.);
#2561=ORIENTED_EDGE('',*,*,#1870,.T.);
#2562=ORIENTED_EDGE('',*,*,#1867,.T.);
#2563=ORIENTED_EDGE('',*,*,#1832,.T.);
#2564=ORIENTED_EDGE('',*,*,#1829,.F.);
#2565=ORIENTED_EDGE('',*,*,#1826,.F.);
#2566=ORIENTED_EDGE('',*,*,#1823,.T.);
#2567=ORIENTED_EDGE('',*,*,#1815,.T.);
#2568=ORIENTED_EDGE('',*,*,#1812,.F.);
#2569=ORIENTED_EDGE('',*,*,#1786,.T.);
#2570=ORIENTED_EDGE('',*,*,#1773,.T.);
#2571=ORIENTED_EDGE('',*,*,#1784,.T.);
#2572=ORIENTED_EDGE('',*,*,#1791,.T.);
#2573=ORIENTED_EDGE('',*,*,#1792,.T.);
#2574=ORIENTED_EDGE('',*,*,#1795,.T.);
#2575=ORIENTED_EDGE('',*,*,#1798,.T.);
#2576=ORIENTED_EDGE('',*,*,#1753,.T.);
#2577=ORIENTED_EDGE('',*,*,#1757,.T.);
#2578=ORIENTED_EDGE('',*,*,#1748,.T.);
#2579=ORIENTED_EDGE('',*,*,#1733,.T.);
#2580=ORIENTED_EDGE('',*,*,#1923,.T.);
#2581=ORIENTED_EDGE('',*,*,#1888,.T.);
#2582=ORIENTED_EDGE('',*,*,#1884,.T.);
#2583=ORIENTED_EDGE('',*,*,#1924,.T.);
#2584=ORIENTED_EDGE('',*,*,#1839,.T.);
#2585=ORIENTED_EDGE('',*,*,#1835,.T.);
#2586=ORIENTED_EDGE('',*,*,#1892,.F.);
#2587=ORIENTED_EDGE('',*,*,#1889,.F.);
#2588=ORIENTED_EDGE('',*,*,#1923,.F.);
#2589=ORIENTED_EDGE('',*,*,#1838,.T.);
#2590=ORIENTED_EDGE('',*,*,#1924,.F.);
#2591=ORIENTED_EDGE('',*,*,#1887,.T.);
#2592=ORIENTED_EDGE('',*,*,#1891,.F.);
#2593=ORIENTED_EDGE('',*,*,#1876,.T.);
#2594=ORIENTED_EDGE('',*,*,#1925,.F.);
#2595=ORIENTED_EDGE('',*,*,#1900,.T.);
#2596=ORIENTED_EDGE('',*,*,#1926,.T.);
#2597=ORIENTED_EDGE('',*,*,#1927,.T.);
#2598=ORIENTED_EDGE('',*,*,#1928,.T.);
#2599=ORIENTED_EDGE('',*,*,#1846,.T.);
#2600=ORIENTED_EDGE('',*,*,#1929,.F.);
#2601=ORIENTED_EDGE('',*,*,#1842,.F.);
#2602=ORIENTED_EDGE('',*,*,#1893,.F.);
#2603=ORIENTED_EDGE('',*,*,#1840,.F.);
#2604=ORIENTED_EDGE('',*,*,#1927,.F.);
#2605=ORIENTED_EDGE('',*,*,#1918,.F.);
#2606=ORIENTED_EDGE('',*,*,#1930,.F.);
#2607=ORIENTED_EDGE('',*,*,#1864,.F.);
#2608=ORIENTED_EDGE('',*,*,#1709,.T.);
#2609=ORIENTED_EDGE('',*,*,#1710,.T.);
#2610=ORIENTED_EDGE('',*,*,#1705,.T.);
#2611=ORIENTED_EDGE('',*,*,#1930,.T.);
#2612=ORIENTED_EDGE('',*,*,#1917,.F.);
#2613=ORIENTED_EDGE('',*,*,#1931,.T.);
#2614=ORIENTED_EDGE('',*,*,#1859,.F.);
#2615=ORIENTED_EDGE('',*,*,#1931,.F.);
#2616=ORIENTED_EDGE('',*,*,#1922,.F.);
#2617=ORIENTED_EDGE('',*,*,#1932,.T.);
#2618=ORIENTED_EDGE('',*,*,#1860,.F.);
#2619=ORIENTED_EDGE('',*,*,#1932,.F.);
#2620=ORIENTED_EDGE('',*,*,#1921,.F.);
#2621=ORIENTED_EDGE('',*,*,#1933,.T.);
#2622=ORIENTED_EDGE('',*,*,#1861,.F.);
#2623=ORIENTED_EDGE('',*,*,#1933,.F.);
#2624=ORIENTED_EDGE('',*,*,#1920,.F.);
#2625=ORIENTED_EDGE('',*,*,#1934,.F.);
#2626=ORIENTED_EDGE('',*,*,#1862,.F.);
#2627=ORIENTED_EDGE('',*,*,#1707,.T.);
#2628=ORIENTED_EDGE('',*,*,#1934,.T.);
#2629=ORIENTED_EDGE('',*,*,#1919,.T.);
#2630=ORIENTED_EDGE('',*,*,#1926,.F.);
#2631=ORIENTED_EDGE('',*,*,#1899,.F.);
#2632=ORIENTED_EDGE('',*,*,#1935,.F.);
#2633=ORIENTED_EDGE('',*,*,#1847,.F.);
#2634=ORIENTED_EDGE('',*,*,#1928,.F.);
#2635=ORIENTED_EDGE('',*,*,#1863,.T.);
#2636=ORIENTED_EDGE('',*,*,#1935,.T.);
#2637=ORIENTED_EDGE('',*,*,#1898,.F.);
#2638=ORIENTED_EDGE('',*,*,#1936,.F.);
#2639=ORIENTED_EDGE('',*,*,#1848,.T.);
#2640=ORIENTED_EDGE('',*,*,#1936,.T.);
#2641=ORIENTED_EDGE('',*,*,#1897,.T.);
#2642=ORIENTED_EDGE('',*,*,#1925,.T.);
#2643=ORIENTED_EDGE('',*,*,#1875,.T.);
#2644=ORIENTED_EDGE('',*,*,#1880,.T.);
#2645=ORIENTED_EDGE('',*,*,#1905,.T.);
#2646=ORIENTED_EDGE('',*,*,#1907,.T.);
#2647=ORIENTED_EDGE('',*,*,#1849,.T.);
#2648=ORIENTED_EDGE('',*,*,#1882,.T.);
#2649=ORIENTED_EDGE('',*,*,#1843,.T.);
#2650=ORIENTED_EDGE('',*,*,#1929,.T.);
#2651=ORIENTED_EDGE('',*,*,#1845,.T.);
#2652=ORIENTED_EDGE('',*,*,#1724,.T.);
#2653=ORIENTED_EDGE('',*,*,#1896,.T.);
#2654=ORIENTED_EDGE('',*,*,#1937,.F.);
#2655=ORIENTED_EDGE('',*,*,#1938,.T.);
#2656=ORIENTED_EDGE('',*,*,#1939,.F.);
#2657=ORIENTED_EDGE('',*,*,#1940,.F.);
#2658=ORIENTED_EDGE('',*,*,#1941,.F.);
#2659=ORIENTED_EDGE('',*,*,#1942,.T.);
#2660=ORIENTED_EDGE('',*,*,#1943,.F.);
#2661=ORIENTED_EDGE('',*,*,#1938,.F.);
#2662=ORIENTED_EDGE('',*,*,#1944,.F.);
#2663=ORIENTED_EDGE('',*,*,#1942,.F.);
#2664=ORIENTED_EDGE('',*,*,#1945,.F.);
#2665=ORIENTED_EDGE('',*,*,#1946,.T.);
#2666=ORIENTED_EDGE('',*,*,#1947,.F.);
#2667=ORIENTED_EDGE('',*,*,#1948,.F.);
#2668=ORIENTED_EDGE('',*,*,#1949,.F.);
#2669=ORIENTED_EDGE('',*,*,#1946,.F.);
#2670=ORIENTED_EDGE('',*,*,#1947,.T.);
#2671=ORIENTED_EDGE('',*,*,#1949,.T.);
#2672=ORIENTED_EDGE('',*,*,#1950,.F.);
#2673=ORIENTED_EDGE('',*,*,#1951,.F.);
#2674=ORIENTED_EDGE('',*,*,#1952,.F.);
#2675=ORIENTED_EDGE('',*,*,#1953,.F.);
#2676=ORIENTED_EDGE('',*,*,#1954,.F.);
#2677=ORIENTED_EDGE('',*,*,#1939,.T.);
#2678=ORIENTED_EDGE('',*,*,#1941,.T.);
#2679=ORIENTED_EDGE('',*,*,#1955,.T.);
#2680=ORIENTED_EDGE('',*,*,#1956,.F.);
#2681=ORIENTED_EDGE('',*,*,#1957,.F.);
#2682=ORIENTED_EDGE('',*,*,#1958,.F.);
#2683=ORIENTED_EDGE('',*,*,#1959,.T.);
#2684=ORIENTED_EDGE('',*,*,#1960,.F.);
#2685=ORIENTED_EDGE('',*,*,#1961,.T.);
#2686=ORIENTED_EDGE('',*,*,#1962,.F.);
#2687=ORIENTED_EDGE('',*,*,#1961,.F.);
#2688=ORIENTED_EDGE('',*,*,#1963,.F.);
#2689=ORIENTED_EDGE('',*,*,#1964,.T.);
#2690=ORIENTED_EDGE('',*,*,#1965,.T.);
#2691=ORIENTED_EDGE('',*,*,#1964,.F.);
#2692=ORIENTED_EDGE('',*,*,#1965,.F.);
#2693=ORIENTED_EDGE('',*,*,#1966,.F.);
#2694=ORIENTED_EDGE('',*,*,#1967,.T.);
#2695=ORIENTED_EDGE('',*,*,#1968,.T.);
#2696=ORIENTED_EDGE('',*,*,#1967,.F.);
#2697=ORIENTED_EDGE('',*,*,#1968,.F.);
#2698=ORIENTED_EDGE('',*,*,#1969,.F.);
#2699=ORIENTED_EDGE('',*,*,#1970,.T.);
#2700=ORIENTED_EDGE('',*,*,#1971,.F.);
#2701=ORIENTED_EDGE('',*,*,#1972,.F.);
#2702=ORIENTED_EDGE('',*,*,#1973,.F.);
#2703=ORIENTED_EDGE('',*,*,#1974,.T.);
#2704=ORIENTED_EDGE('',*,*,#1975,.F.);
#2705=ORIENTED_EDGE('',*,*,#1976,.F.);
#2706=ORIENTED_EDGE('',*,*,#1970,.F.);
#2707=ORIENTED_EDGE('',*,*,#1977,.F.);
#2708=ORIENTED_EDGE('',*,*,#1978,.T.);
#2709=ORIENTED_EDGE('',*,*,#1979,.F.);
#2710=ORIENTED_EDGE('',*,*,#1980,.F.);
#2711=ORIENTED_EDGE('',*,*,#1981,.F.);
#2712=ORIENTED_EDGE('',*,*,#1982,.T.);
#2713=ORIENTED_EDGE('',*,*,#1983,.F.);
#2714=ORIENTED_EDGE('',*,*,#1978,.F.);
#2715=ORIENTED_EDGE('',*,*,#1984,.F.);
#2716=ORIENTED_EDGE('',*,*,#1985,.T.);
#2717=ORIENTED_EDGE('',*,*,#1986,.F.);
#2718=ORIENTED_EDGE('',*,*,#1985,.F.);
#2719=ORIENTED_EDGE('',*,*,#1984,.T.);
#2720=ORIENTED_EDGE('',*,*,#1987,.F.);
#2721=ORIENTED_EDGE('',*,*,#1988,.T.);
#2722=ORIENTED_EDGE('',*,*,#1989,.T.);
#2723=ORIENTED_EDGE('',*,*,#1990,.F.);
#2724=ORIENTED_EDGE('',*,*,#1991,.F.);
#2725=ORIENTED_EDGE('',*,*,#1992,.F.);
#2726=ORIENTED_EDGE('',*,*,#1993,.T.);
#2727=ORIENTED_EDGE('',*,*,#1994,.F.);
#2728=ORIENTED_EDGE('',*,*,#1995,.T.);
#2729=ORIENTED_EDGE('',*,*,#1996,.T.);
#2730=ORIENTED_EDGE('',*,*,#1997,.T.);
#2731=ORIENTED_EDGE('',*,*,#1958,.T.);
#2732=ORIENTED_EDGE('',*,*,#1998,.F.);
#2733=ORIENTED_EDGE('',*,*,#1999,.T.);
#2734=ORIENTED_EDGE('',*,*,#2000,.T.);
#2735=ORIENTED_EDGE('',*,*,#2001,.T.);
#2736=ORIENTED_EDGE('',*,*,#2002,.F.);
#2737=ORIENTED_EDGE('',*,*,#1951,.T.);
#2738=ORIENTED_EDGE('',*,*,#2003,.T.);
#2739=ORIENTED_EDGE('',*,*,#2004,.T.);
#2740=ORIENTED_EDGE('',*,*,#2005,.F.);
#2741=ORIENTED_EDGE('',*,*,#2006,.T.);
#2742=ORIENTED_EDGE('',*,*,#2007,.F.);
#2743=ORIENTED_EDGE('',*,*,#2008,.F.);
#2744=ORIENTED_EDGE('',*,*,#2009,.F.);
#2745=ORIENTED_EDGE('',*,*,#2010,.T.);
#2746=ORIENTED_EDGE('',*,*,#2011,.T.);
#2747=ORIENTED_EDGE('',*,*,#2012,.F.);
#2748=ORIENTED_EDGE('',*,*,#2013,.F.);
#2749=ORIENTED_EDGE('',*,*,#2014,.T.);
#2750=ORIENTED_EDGE('',*,*,#2015,.T.);
#2751=ORIENTED_EDGE('',*,*,#2016,.F.);
#2752=ORIENTED_EDGE('',*,*,#2011,.F.);
#2753=ORIENTED_EDGE('',*,*,#2017,.F.);
#2754=ORIENTED_EDGE('',*,*,#2018,.T.);
#2755=ORIENTED_EDGE('',*,*,#2019,.F.);
#2756=ORIENTED_EDGE('',*,*,#2015,.F.);
#2757=ORIENTED_EDGE('',*,*,#2020,.F.);
#2758=ORIENTED_EDGE('',*,*,#2021,.T.);
#2759=ORIENTED_EDGE('',*,*,#2022,.F.);
#2760=ORIENTED_EDGE('',*,*,#1982,.F.);
#2761=ORIENTED_EDGE('',*,*,#2023,.F.);
#2762=ORIENTED_EDGE('',*,*,#2024,.T.);
#2763=ORIENTED_EDGE('',*,*,#2025,.F.);
#2764=ORIENTED_EDGE('',*,*,#2021,.F.);
#2765=ORIENTED_EDGE('',*,*,#2026,.F.);
#2766=ORIENTED_EDGE('',*,*,#2027,.T.);
#2767=ORIENTED_EDGE('',*,*,#2028,.F.);
#2768=ORIENTED_EDGE('',*,*,#2024,.F.);
#2769=ORIENTED_EDGE('',*,*,#2029,.T.);
#2770=ORIENTED_EDGE('',*,*,#2030,.T.);
#2771=ORIENTED_EDGE('',*,*,#2031,.T.);
#2772=ORIENTED_EDGE('',*,*,#2032,.F.);
#2773=ORIENTED_EDGE('',*,*,#2033,.F.);
#2774=ORIENTED_EDGE('',*,*,#2034,.F.);
#2775=ORIENTED_EDGE('',*,*,#2027,.F.);
#2776=ORIENTED_EDGE('',*,*,#2035,.F.);
#2777=ORIENTED_EDGE('',*,*,#1980,.T.);
#2778=ORIENTED_EDGE('',*,*,#2036,.F.);
#2779=ORIENTED_EDGE('',*,*,#1976,.T.);
#2780=ORIENTED_EDGE('',*,*,#2037,.F.);
#2781=ORIENTED_EDGE('',*,*,#1990,.T.);
#2782=ORIENTED_EDGE('',*,*,#2038,.T.);
#2783=ORIENTED_EDGE('',*,*,#2008,.T.);
#2784=ORIENTED_EDGE('',*,*,#2033,.T.);
#2785=ORIENTED_EDGE('',*,*,#2039,.F.);
#2786=ORIENTED_EDGE('',*,*,#2040,.F.);
#2787=ORIENTED_EDGE('',*,*,#2041,.T.);
#2788=ORIENTED_EDGE('',*,*,#2042,.T.);
#2789=ORIENTED_EDGE('',*,*,#2043,.T.);
#2790=ORIENTED_EDGE('',*,*,#2039,.T.);
#2791=ORIENTED_EDGE('',*,*,#2032,.T.);
#2792=ORIENTED_EDGE('',*,*,#2044,.T.);
#2793=ORIENTED_EDGE('',*,*,#2045,.T.);
#2794=ORIENTED_EDGE('',*,*,#1987,.T.);
#2795=ORIENTED_EDGE('',*,*,#2037,.T.);
#2796=ORIENTED_EDGE('',*,*,#1975,.T.);
#2797=ORIENTED_EDGE('',*,*,#2046,.T.);
#2798=ORIENTED_EDGE('',*,*,#1991,.T.);
#2799=ORIENTED_EDGE('',*,*,#1986,.T.);
#2800=ORIENTED_EDGE('',*,*,#1963,.T.);
#2801=ORIENTED_EDGE('',*,*,#2044,.F.);
#2802=ORIENTED_EDGE('',*,*,#2031,.F.);
#2803=ORIENTED_EDGE('',*,*,#2047,.T.);
#2804=ORIENTED_EDGE('',*,*,#2048,.F.);
#2805=ORIENTED_EDGE('',*,*,#2045,.F.);
#2806=ORIENTED_EDGE('',*,*,#2048,.T.);
#2807=ORIENTED_EDGE('',*,*,#2049,.T.);
#2808=ORIENTED_EDGE('',*,*,#1988,.F.);
#2809=ORIENTED_EDGE('',*,*,#2042,.F.);
#2810=ORIENTED_EDGE('',*,*,#2050,.T.);
#2811=ORIENTED_EDGE('',*,*,#2051,.T.);
#2812=ORIENTED_EDGE('',*,*,#2052,.F.);
#2813=ORIENTED_EDGE('',*,*,#2053,.T.);
#2814=ORIENTED_EDGE('',*,*,#2054,.T.);
#2815=ORIENTED_EDGE('',*,*,#2055,.F.);
#2816=ORIENTED_EDGE('',*,*,#1956,.T.);
#2817=ORIENTED_EDGE('',*,*,#2056,.T.);
#2818=ORIENTED_EDGE('',*,*,#2057,.T.);
#2819=ORIENTED_EDGE('',*,*,#2049,.F.);
#2820=ORIENTED_EDGE('',*,*,#2047,.F.);
#2821=ORIENTED_EDGE('',*,*,#2030,.F.);
#2822=ORIENTED_EDGE('',*,*,#2058,.T.);
#2823=ORIENTED_EDGE('',*,*,#1952,.T.);
#2824=ORIENTED_EDGE('',*,*,#2002,.T.);
#2825=ORIENTED_EDGE('',*,*,#2038,.F.);
#2826=ORIENTED_EDGE('',*,*,#1989,.F.);
#2827=ORIENTED_EDGE('',*,*,#2059,.T.);
#2828=ORIENTED_EDGE('',*,*,#2060,.T.);
#2829=ORIENTED_EDGE('',*,*,#2061,.T.);
#2830=ORIENTED_EDGE('',*,*,#1953,.T.);
#2831=ORIENTED_EDGE('',*,*,#2058,.F.);
#2832=ORIENTED_EDGE('',*,*,#2062,.T.);
#2833=ORIENTED_EDGE('',*,*,#2063,.T.);
#2834=ORIENTED_EDGE('',*,*,#2059,.F.);
#2835=ORIENTED_EDGE('',*,*,#2064,.T.);
#2836=ORIENTED_EDGE('',*,*,#2000,.F.);
#2837=ORIENTED_EDGE('',*,*,#2065,.T.);
#2838=ORIENTED_EDGE('',*,*,#2060,.F.);
#2839=ORIENTED_EDGE('',*,*,#2063,.F.);
#2840=ORIENTED_EDGE('',*,*,#2004,.F.);
#2841=ORIENTED_EDGE('',*,*,#1948,.T.);
#2842=ORIENTED_EDGE('',*,*,#1954,.T.);
#2843=ORIENTED_EDGE('',*,*,#2061,.F.);
#2844=ORIENTED_EDGE('',*,*,#2065,.F.);
#2845=ORIENTED_EDGE('',*,*,#2003,.F.);
#2846=ORIENTED_EDGE('',*,*,#1950,.T.);
#2847=ORIENTED_EDGE('',*,*,#2064,.F.);
#2848=ORIENTED_EDGE('',*,*,#2062,.F.);
#2849=ORIENTED_EDGE('',*,*,#2029,.F.);
#2850=ORIENTED_EDGE('',*,*,#2001,.F.);
#2851=ORIENTED_EDGE('',*,*,#1945,.T.);
#2852=ORIENTED_EDGE('',*,*,#2066,.F.);
#2853=ORIENTED_EDGE('',*,*,#2018,.F.);
#2854=ORIENTED_EDGE('',*,*,#2067,.F.);
#2855=ORIENTED_EDGE('',*,*,#1972,.T.);
#2856=ORIENTED_EDGE('',*,*,#2068,.T.);
#2857=ORIENTED_EDGE('',*,*,#2009,.T.);
#2858=ORIENTED_EDGE('',*,*,#2040,.T.);
#2859=ORIENTED_EDGE('',*,*,#2043,.F.);
#2860=ORIENTED_EDGE('',*,*,#2052,.T.);
#2861=ORIENTED_EDGE('',*,*,#2069,.T.);
#2862=ORIENTED_EDGE('',*,*,#2070,.T.);
#2863=ORIENTED_EDGE('',*,*,#2071,.T.);
#2864=ORIENTED_EDGE('',*,*,#1992,.T.);
#2865=ORIENTED_EDGE('',*,*,#2046,.F.);
#2866=ORIENTED_EDGE('',*,*,#1974,.F.);
#2867=ORIENTED_EDGE('',*,*,#2070,.F.);
#2868=ORIENTED_EDGE('',*,*,#2054,.F.);
#2869=ORIENTED_EDGE('',*,*,#2072,.F.);
#2870=ORIENTED_EDGE('',*,*,#1999,.F.);
#2871=ORIENTED_EDGE('',*,*,#1943,.T.);
#2872=ORIENTED_EDGE('',*,*,#1944,.T.);
#2873=ORIENTED_EDGE('',*,*,#1937,.T.);
#2874=ORIENTED_EDGE('',*,*,#2072,.T.);
#2875=ORIENTED_EDGE('',*,*,#2053,.F.);
#2876=ORIENTED_EDGE('',*,*,#2073,.T.);
#2877=ORIENTED_EDGE('',*,*,#1995,.F.);
#2878=ORIENTED_EDGE('',*,*,#2073,.F.);
#2879=ORIENTED_EDGE('',*,*,#2057,.F.);
#2880=ORIENTED_EDGE('',*,*,#2074,.F.);
#2881=ORIENTED_EDGE('',*,*,#1996,.F.);
#2882=ORIENTED_EDGE('',*,*,#1940,.T.);
#2883=ORIENTED_EDGE('',*,*,#1959,.F.);
#2884=ORIENTED_EDGE('',*,*,#1997,.F.);
#2885=ORIENTED_EDGE('',*,*,#2074,.T.);
#2886=ORIENTED_EDGE('',*,*,#2056,.F.);
#2887=ORIENTED_EDGE('',*,*,#1955,.F.);
#2888=ORIENTED_EDGE('',*,*,#1957,.T.);
#2889=ORIENTED_EDGE('',*,*,#2055,.T.);
#2890=ORIENTED_EDGE('',*,*,#2069,.F.);
#2891=ORIENTED_EDGE('',*,*,#2051,.F.);
#2892=ORIENTED_EDGE('',*,*,#2075,.F.);
#2893=ORIENTED_EDGE('',*,*,#1993,.F.);
#2894=ORIENTED_EDGE('',*,*,#2071,.F.);
#2895=ORIENTED_EDGE('',*,*,#1998,.T.);
#2896=ORIENTED_EDGE('',*,*,#2075,.T.);
#2897=ORIENTED_EDGE('',*,*,#2050,.F.);
#2898=ORIENTED_EDGE('',*,*,#2041,.F.);
#2899=ORIENTED_EDGE('',*,*,#1994,.T.);
#2900=ORIENTED_EDGE('',*,*,#2076,.F.);
#2901=ORIENTED_EDGE('',*,*,#2077,.F.);
#2902=ORIENTED_EDGE('',*,*,#2078,.F.);
#2903=ORIENTED_EDGE('',*,*,#2079,.F.);
#2904=ORIENTED_EDGE('',*,*,#2080,.F.);
#2905=ORIENTED_EDGE('',*,*,#2081,.F.);
#2906=ORIENTED_EDGE('',*,*,#2082,.F.);
#2907=ORIENTED_EDGE('',*,*,#2083,.F.);
#2908=ORIENTED_EDGE('',*,*,#2084,.F.);
#2909=ORIENTED_EDGE('',*,*,#2085,.F.);
#2910=ORIENTED_EDGE('',*,*,#2086,.F.);
#2911=ORIENTED_EDGE('',*,*,#2087,.T.);
#2912=ORIENTED_EDGE('',*,*,#2083,.T.);
#2913=ORIENTED_EDGE('',*,*,#2088,.F.);
#2914=ORIENTED_EDGE('',*,*,#2089,.F.);
#2915=ORIENTED_EDGE('',*,*,#2090,.F.);
#2916=ORIENTED_EDGE('',*,*,#2091,.T.);
#2917=ORIENTED_EDGE('',*,*,#2092,.T.);
#2918=ORIENTED_EDGE('',*,*,#2092,.F.);
#2919=ORIENTED_EDGE('',*,*,#2093,.T.);
#2920=ORIENTED_EDGE('',*,*,#2094,.F.);
#2921=ORIENTED_EDGE('',*,*,#2093,.F.);
#2922=ORIENTED_EDGE('',*,*,#2081,.T.);
#2923=ORIENTED_EDGE('',*,*,#2095,.F.);
#2924=ORIENTED_EDGE('',*,*,#2096,.T.);
#2925=ORIENTED_EDGE('',*,*,#2097,.F.);
#2926=ORIENTED_EDGE('',*,*,#2098,.T.);
#2927=ORIENTED_EDGE('',*,*,#2099,.F.);
#2928=ORIENTED_EDGE('',*,*,#2100,.F.);
#2929=ORIENTED_EDGE('',*,*,#2101,.T.);
#2930=ORIENTED_EDGE('',*,*,#2102,.F.);
#2931=ORIENTED_EDGE('',*,*,#2103,.F.);
#2932=ORIENTED_EDGE('',*,*,#2104,.F.);
#2933=ORIENTED_EDGE('',*,*,#2103,.T.);
#2934=ORIENTED_EDGE('',*,*,#2105,.F.);
#2935=ORIENTED_EDGE('',*,*,#2096,.F.);
#2936=ORIENTED_EDGE('',*,*,#2106,.F.);
#2937=ORIENTED_EDGE('',*,*,#2090,.T.);
#2938=ORIENTED_EDGE('',*,*,#2089,.T.);
#2939=ORIENTED_EDGE('',*,*,#2107,.F.);
#2940=ORIENTED_EDGE('',*,*,#2098,.F.);
#2941=ORIENTED_EDGE('',*,*,#2108,.F.);
#2942=ORIENTED_EDGE('',*,*,#2109,.T.);
#2943=ORIENTED_EDGE('',*,*,#2108,.T.);
#2944=ORIENTED_EDGE('',*,*,#2110,.F.);
#2945=ORIENTED_EDGE('',*,*,#2111,.F.);
#2946=ORIENTED_EDGE('',*,*,#2112,.F.);
#2947=ORIENTED_EDGE('',*,*,#2113,.T.);
#2948=ORIENTED_EDGE('',*,*,#2114,.F.);
#2949=ORIENTED_EDGE('',*,*,#2085,.T.);
#2950=ORIENTED_EDGE('',*,*,#2114,.T.);
#2951=ORIENTED_EDGE('',*,*,#2115,.T.);
#2952=ORIENTED_EDGE('',*,*,#2116,.F.);
#2953=ORIENTED_EDGE('',*,*,#2086,.T.);
#2954=ORIENTED_EDGE('',*,*,#2117,.F.);
#2955=ORIENTED_EDGE('',*,*,#2118,.T.);
#2956=ORIENTED_EDGE('',*,*,#2119,.T.);
#2957=ORIENTED_EDGE('',*,*,#2078,.T.);
#2958=ORIENTED_EDGE('',*,*,#2119,.F.);
#2959=ORIENTED_EDGE('',*,*,#2120,.T.);
#2960=ORIENTED_EDGE('',*,*,#2121,.F.);
#2961=ORIENTED_EDGE('',*,*,#2079,.T.);
#2962=ORIENTED_EDGE('',*,*,#2067,.T.);
#2963=ORIENTED_EDGE('',*,*,#2017,.T.);
#2964=ORIENTED_EDGE('',*,*,#2014,.F.);
#2965=ORIENTED_EDGE('',*,*,#2010,.F.);
#2966=ORIENTED_EDGE('',*,*,#2122,.T.);
#2967=ORIENTED_EDGE('',*,*,#2123,.T.);
#2968=ORIENTED_EDGE('',*,*,#2124,.F.);
#2969=ORIENTED_EDGE('',*,*,#2125,.T.);
#2970=ORIENTED_EDGE('',*,*,#2112,.T.);
#2971=ORIENTED_EDGE('',*,*,#2084,.T.);
#2972=ORIENTED_EDGE('',*,*,#2091,.F.);
#2973=ORIENTED_EDGE('',*,*,#2106,.T.);
#2974=ORIENTED_EDGE('',*,*,#2109,.F.);
#2975=ORIENTED_EDGE('',*,*,#2126,.T.);
#2976=ORIENTED_EDGE('',*,*,#2127,.T.);
#2977=ORIENTED_EDGE('',*,*,#2128,.T.);
#2978=ORIENTED_EDGE('',*,*,#2129,.F.);
#2979=ORIENTED_EDGE('',*,*,#2130,.F.);
#2980=ORIENTED_EDGE('',*,*,#2131,.F.);
#2981=ORIENTED_EDGE('',*,*,#2005,.T.);
#2982=ORIENTED_EDGE('',*,*,#2068,.F.);
#2983=ORIENTED_EDGE('',*,*,#1973,.T.);
#2984=ORIENTED_EDGE('',*,*,#1969,.T.);
#2985=ORIENTED_EDGE('',*,*,#2121,.T.);
#2986=ORIENTED_EDGE('',*,*,#2132,.T.);
#2987=ORIENTED_EDGE('',*,*,#2133,.T.);
#2988=ORIENTED_EDGE('',*,*,#2134,.T.);
#2989=ORIENTED_EDGE('',*,*,#2135,.T.);
#2990=ORIENTED_EDGE('',*,*,#2136,.T.);
#2991=ORIENTED_EDGE('',*,*,#2100,.T.);
#2992=ORIENTED_EDGE('',*,*,#2104,.T.);
#2993=ORIENTED_EDGE('',*,*,#2095,.T.);
#2994=ORIENTED_EDGE('',*,*,#2080,.T.);
#2995=ORIENTED_EDGE('',*,*,#2020,.T.);
#2996=ORIENTED_EDGE('',*,*,#1981,.T.);
#2997=ORIENTED_EDGE('',*,*,#1977,.T.);
#2998=ORIENTED_EDGE('',*,*,#2035,.T.);
#2999=ORIENTED_EDGE('',*,*,#2026,.T.);
#3000=ORIENTED_EDGE('',*,*,#2023,.T.);
#3001=ORIENTED_EDGE('',*,*,#2117,.T.);
#3002=ORIENTED_EDGE('',*,*,#2077,.T.);
#3003=ORIENTED_EDGE('',*,*,#2137,.F.);
#3004=ORIENTED_EDGE('',*,*,#2138,.F.);
#3005=ORIENTED_EDGE('',*,*,#1962,.T.);
#3006=ORIENTED_EDGE('',*,*,#2139,.T.);
#3007=ORIENTED_EDGE('',*,*,#2140,.T.);
#3008=ORIENTED_EDGE('',*,*,#2141,.T.);
#3009=ORIENTED_EDGE('',*,*,#2142,.T.);
#3010=ORIENTED_EDGE('',*,*,#2143,.T.);
#3011=ORIENTED_EDGE('',*,*,#2144,.T.);
#3012=ORIENTED_EDGE('',*,*,#2137,.T.);
#3013=ORIENTED_EDGE('',*,*,#2076,.T.);
#3014=ORIENTED_EDGE('',*,*,#2099,.T.);
#3015=ORIENTED_EDGE('',*,*,#2107,.T.);
#3016=ORIENTED_EDGE('',*,*,#2088,.T.);
#3017=ORIENTED_EDGE('',*,*,#2082,.T.);
#3018=ORIENTED_EDGE('',*,*,#2094,.T.);
#3019=ORIENTED_EDGE('',*,*,#1966,.T.);
#3020=ORIENTED_EDGE('',*,*,#2145,.F.);
#3021=ORIENTED_EDGE('',*,*,#2146,.F.);
#3022=ORIENTED_EDGE('',*,*,#2122,.F.);
#3023=ORIENTED_EDGE('',*,*,#2013,.T.);
#3024=ORIENTED_EDGE('',*,*,#2147,.F.);
#3025=ORIENTED_EDGE('',*,*,#2148,.F.);
#3026=ORIENTED_EDGE('',*,*,#2126,.F.);
#3027=ORIENTED_EDGE('',*,*,#2111,.T.);
#3028=ORIENTED_EDGE('',*,*,#2149,.T.);
#3029=ORIENTED_EDGE('',*,*,#2150,.T.);
#3030=ORIENTED_EDGE('',*,*,#2151,.T.);
#3031=ORIENTED_EDGE('',*,*,#2152,.T.);
#3032=ORIENTED_EDGE('',*,*,#2153,.T.);
#3033=ORIENTED_EDGE('',*,*,#2147,.T.);
#3034=ORIENTED_EDGE('',*,*,#2110,.T.);
#3035=ORIENTED_EDGE('',*,*,#2097,.T.);
#3036=ORIENTED_EDGE('',*,*,#2105,.T.);
#3037=ORIENTED_EDGE('',*,*,#2102,.T.);
#3038=ORIENTED_EDGE('',*,*,#2154,.T.);
#3039=ORIENTED_EDGE('',*,*,#2155,.T.);
#3040=ORIENTED_EDGE('',*,*,#2156,.T.);
#3041=ORIENTED_EDGE('',*,*,#2157,.T.);
#3042=ORIENTED_EDGE('',*,*,#2158,.T.);
#3043=ORIENTED_EDGE('',*,*,#2145,.T.);
#3044=ORIENTED_EDGE('',*,*,#2012,.T.);
#3045=ORIENTED_EDGE('',*,*,#2016,.T.);
#3046=ORIENTED_EDGE('',*,*,#2019,.T.);
#3047=ORIENTED_EDGE('',*,*,#2066,.T.);
#3048=ORIENTED_EDGE('',*,*,#1971,.T.);
#3049=ORIENTED_EDGE('',*,*,#2036,.T.);
#3050=ORIENTED_EDGE('',*,*,#1979,.T.);
#3051=ORIENTED_EDGE('',*,*,#1983,.T.);
#3052=ORIENTED_EDGE('',*,*,#2022,.T.);
#3053=ORIENTED_EDGE('',*,*,#2025,.T.);
#3054=ORIENTED_EDGE('',*,*,#2028,.T.);
#3055=ORIENTED_EDGE('',*,*,#2034,.T.);
#3056=ORIENTED_EDGE('',*,*,#2007,.T.);
#3057=ORIENTED_EDGE('',*,*,#2144,.F.);
#3058=ORIENTED_EDGE('',*,*,#2159,.F.);
#3059=ORIENTED_EDGE('',*,*,#2132,.F.);
#3060=ORIENTED_EDGE('',*,*,#2120,.F.);
#3061=ORIENTED_EDGE('',*,*,#2118,.F.);
#3062=ORIENTED_EDGE('',*,*,#2138,.T.);
#3063=ORIENTED_EDGE('',*,*,#2116,.T.);
#3064=ORIENTED_EDGE('',*,*,#2160,.T.);
#3065=ORIENTED_EDGE('',*,*,#2139,.F.);
#3066=ORIENTED_EDGE('',*,*,#2087,.F.);
#3067=ORIENTED_EDGE('',*,*,#1960,.T.);
#3068=ORIENTED_EDGE('',*,*,#2140,.F.);
#3069=ORIENTED_EDGE('',*,*,#2160,.F.);
#3070=ORIENTED_EDGE('',*,*,#2115,.F.);
#3071=ORIENTED_EDGE('',*,*,#2113,.F.);
#3072=ORIENTED_EDGE('',*,*,#2125,.F.);
#3073=ORIENTED_EDGE('',*,*,#2161,.F.);
#3074=ORIENTED_EDGE('',*,*,#2159,.T.);
#3075=ORIENTED_EDGE('',*,*,#2143,.F.);
#3076=ORIENTED_EDGE('',*,*,#2162,.F.);
#3077=ORIENTED_EDGE('',*,*,#2157,.F.);
#3078=ORIENTED_EDGE('',*,*,#2163,.F.);
#3079=ORIENTED_EDGE('',*,*,#2133,.F.);
#3080=ORIENTED_EDGE('',*,*,#2134,.F.);
#3081=ORIENTED_EDGE('',*,*,#2163,.T.);
#3082=ORIENTED_EDGE('',*,*,#2156,.F.);
#3083=ORIENTED_EDGE('',*,*,#2164,.F.);
#3084=ORIENTED_EDGE('',*,*,#2135,.F.);
#3085=ORIENTED_EDGE('',*,*,#2164,.T.);
#3086=ORIENTED_EDGE('',*,*,#2155,.F.);
#3087=ORIENTED_EDGE('',*,*,#2165,.F.);
#3088=ORIENTED_EDGE('',*,*,#2136,.F.);
#3089=ORIENTED_EDGE('',*,*,#2165,.T.);
#3090=ORIENTED_EDGE('',*,*,#2154,.F.);
#3091=ORIENTED_EDGE('',*,*,#2101,.F.);
#3092=ORIENTED_EDGE('',*,*,#2127,.F.);
#3093=ORIENTED_EDGE('',*,*,#2148,.T.);
#3094=ORIENTED_EDGE('',*,*,#2153,.F.);
#3095=ORIENTED_EDGE('',*,*,#2166,.F.);
#3096=ORIENTED_EDGE('',*,*,#2128,.F.);
#3097=ORIENTED_EDGE('',*,*,#2166,.T.);
#3098=ORIENTED_EDGE('',*,*,#2152,.F.);
#3099=ORIENTED_EDGE('',*,*,#2167,.F.);
#3100=ORIENTED_EDGE('',*,*,#2129,.T.);
#3101=ORIENTED_EDGE('',*,*,#2167,.T.);
#3102=ORIENTED_EDGE('',*,*,#2151,.F.);
#3103=ORIENTED_EDGE('',*,*,#2168,.F.);
#3104=ORIENTED_EDGE('',*,*,#2130,.T.);
#3105=ORIENTED_EDGE('',*,*,#2168,.T.);
#3106=ORIENTED_EDGE('',*,*,#2150,.F.);
#3107=ORIENTED_EDGE('',*,*,#2169,.T.);
#3108=ORIENTED_EDGE('',*,*,#2161,.T.);
#3109=ORIENTED_EDGE('',*,*,#2124,.T.);
#3110=ORIENTED_EDGE('',*,*,#2170,.T.);
#3111=ORIENTED_EDGE('',*,*,#2171,.T.);
#3112=ORIENTED_EDGE('',*,*,#2141,.F.);
#3113=ORIENTED_EDGE('',*,*,#2123,.F.);
#3114=ORIENTED_EDGE('',*,*,#2146,.T.);
#3115=ORIENTED_EDGE('',*,*,#2158,.F.);
#3116=ORIENTED_EDGE('',*,*,#2162,.T.);
#3117=ORIENTED_EDGE('',*,*,#2142,.F.);
#3118=ORIENTED_EDGE('',*,*,#2171,.F.);
#3119=ORIENTED_EDGE('',*,*,#2170,.F.);
#3120=ORIENTED_EDGE('',*,*,#2131,.T.);
#3121=ORIENTED_EDGE('',*,*,#2169,.F.);
#3122=ORIENTED_EDGE('',*,*,#2149,.F.);
#3123=ORIENTED_EDGE('',*,*,#2006,.F.);
#3124=ORIENTED_EDGE('',*,*,#2172,.T.);
#3125=ORIENTED_EDGE('',*,*,#2173,.F.);
#3126=ORIENTED_EDGE('',*,*,#2174,.T.);
#3127=ORIENTED_EDGE('',*,*,#2172,.F.);
#3128=ORIENTED_EDGE('',*,*,#2174,.F.);
#3129=ORIENTED_EDGE('',*,*,#2173,.T.);
#3130=ORIENTED_EDGE('',*,*,#2175,.F.);
#3131=ORIENTED_EDGE('',*,*,#2176,.T.);
#3132=ORIENTED_EDGE('',*,*,#2177,.F.);
#3133=ORIENTED_EDGE('',*,*,#2176,.F.);
#3134=ORIENTED_EDGE('',*,*,#2177,.T.);
#3135=ORIENTED_EDGE('',*,*,#2175,.T.);
#3136=ORIENTED_EDGE('',*,*,#2178,.F.);
#3137=ORIENTED_EDGE('',*,*,#2179,.T.);
#3138=ORIENTED_EDGE('',*,*,#2180,.F.);
#3139=ORIENTED_EDGE('',*,*,#2179,.F.);
#3140=ORIENTED_EDGE('',*,*,#2180,.T.);
#3141=ORIENTED_EDGE('',*,*,#2178,.T.);
#3142=ORIENTED_EDGE('',*,*,#2181,.F.);
#3143=ORIENTED_EDGE('',*,*,#2182,.T.);
#3144=ORIENTED_EDGE('',*,*,#2183,.F.);
#3145=ORIENTED_EDGE('',*,*,#2182,.F.);
#3146=ORIENTED_EDGE('',*,*,#2183,.T.);
#3147=ORIENTED_EDGE('',*,*,#2181,.T.);
#3148=ORIENTED_EDGE('',*,*,#2184,.T.);
#3149=ORIENTED_EDGE('',*,*,#2185,.F.);
#3150=ORIENTED_EDGE('',*,*,#2186,.T.);
#3151=ORIENTED_EDGE('',*,*,#2184,.F.);
#3152=ORIENTED_EDGE('',*,*,#2186,.F.);
#3153=ORIENTED_EDGE('',*,*,#2185,.T.);
#3154=ORIENTED_EDGE('',*,*,#2187,.T.);
#3155=ORIENTED_EDGE('',*,*,#2188,.T.);
#3156=ORIENTED_EDGE('',*,*,#2189,.T.);
#3157=ORIENTED_EDGE('',*,*,#2188,.F.);
#3158=ORIENTED_EDGE('',*,*,#2187,.F.);
#3159=ORIENTED_EDGE('',*,*,#2189,.F.);
#3160=PLANE('',#3569);
#3161=PLANE('',#3583);
#3162=PLANE('',#3587);
#3163=PLANE('',#3591);
#3164=PLANE('',#3592);
#3165=PLANE('',#3593);
#3166=PLANE('',#3594);
#3167=PLANE('',#3595);
#3168=PLANE('',#3599);
#3169=PLANE('',#3600);
#3170=PLANE('',#3607);
#3171=PLANE('',#3608);
#3172=PLANE('',#3609);
#3173=PLANE('',#3610);
#3174=PLANE('',#3611);
#3175=PLANE('',#3612);
#3176=PLANE('',#3617);
#3177=PLANE('',#3618);
#3178=PLANE('',#3619);
#3179=PLANE('',#3620);
#3180=PLANE('',#3624);
#3181=PLANE('',#3628);
#3182=PLANE('',#3632);
#3183=PLANE('',#3636);
#3184=PLANE('',#3644);
#3185=PLANE('',#3648);
#3186=PLANE('',#3652);
#3187=PLANE('',#3658);
#3188=PLANE('',#3659);
#3189=PLANE('',#3660);
#3190=PLANE('',#3661);
#3191=PLANE('',#3662);
#3192=PLANE('',#3666);
#3193=PLANE('',#3670);
#3194=PLANE('',#3674);
#3195=PLANE('',#3675);
#3196=PLANE('',#3680);
#3197=PLANE('',#3681);
#3198=PLANE('',#3682);
#3199=PLANE('',#3683);
#3200=PLANE('',#3684);
#3201=PLANE('',#3685);
#3202=PLANE('',#3686);
#3203=PLANE('',#3687);
#3204=PLANE('',#3688);
#3205=PLANE('',#3689);
#3206=PLANE('',#3690);
#3207=PLANE('',#3691);
#3208=PLANE('',#3692);
#3209=PLANE('',#3695);
#3210=PLANE('',#3696);
#3211=PLANE('',#3697);
#3212=PLANE('',#3698);
#3213=PLANE('',#3699);
#3214=PLANE('',#3700);
#3215=PLANE('',#3701);
#3216=PLANE('',#3702);
#3217=PLANE('',#3703);
#3218=PLANE('',#3705);
#3219=PLANE('',#3718);
#3220=PLANE('',#3719);
#3221=PLANE('',#3726);
#3222=PLANE('',#3730);
#3223=PLANE('',#3731);
#3224=PLANE('',#3738);
#3225=PLANE('',#3742);
#3226=PLANE('',#3743);
#3227=PLANE('',#3744);
#3228=PLANE('',#3745);
#3229=PLANE('',#3746);
#3230=PLANE('',#3754);
#3231=PLANE('',#3761);
#3232=PLANE('',#3765);
#3233=PLANE('',#3768);
#3234=PLANE('',#3769);
#3235=PLANE('',#3770);
#3236=PLANE('',#3771);
#3237=PLANE('',#3772);
#3238=PLANE('',#3773);
#3239=PLANE('',#3774);
#3240=PLANE('',#3775);
#3241=PLANE('',#3776);
#3242=PLANE('',#3777);
#3243=PLANE('',#3778);
#3244=PLANE('',#3782);
#3245=PLANE('',#3783);
#3246=PLANE('',#3784);
#3247=PLANE('',#3785);
#3248=PLANE('',#3786);
#3249=PLANE('',#3787);
#3250=PLANE('',#3788);
#3251=PLANE('',#3789);
#3252=PLANE('',#3790);
#3253=PLANE('',#3791);
#3254=PLANE('',#3792);
#3255=PLANE('',#3796);
#3256=PLANE('',#3797);
#3257=PLANE('',#3804);
#3258=PLANE('',#3805);
#3259=PLANE('',#3806);
#3260=PLANE('',#3807);
#3261=PLANE('',#3808);
#3262=PLANE('',#3809);
#3263=PLANE('',#3816);
#3264=PLANE('',#3817);
#3265=PLANE('',#3819);
#3266=PLANE('',#3822);
#3267=PLANE('',#3828);
#3268=PLANE('',#3829);
#3269=PLANE('',#3830);
#3270=PLANE('',#3831);
#3271=PLANE('',#3833);
#3272=PLANE('',#3835);
#3273=PLANE('',#3837);
#3274=PLANE('',#3839);
#3275=PLANE('',#3841);
#3276=PLANE('',#3843);
#3277=PLANE('',#3847);
#3278=PLANE('',#3852);
#3279=PLANE('',#3853);
#3280=PLANE('',#3858);
#3281=PLANE('',#3859);
#3282=PLANE('',#3864);
#3283=PLANE('',#3865);
#3284=PLANE('',#3867);
#3285=PLANE('',#3871);
#3286=PLANE('',#3876);
#3287=PLANE('',#3877);
#3288=ADVANCED_FACE('',(#168),#3160,.T.);
#3289=ADVANCED_FACE('',(#169),#114,.F.);
#3290=ADVANCED_FACE('',(#170),#115,.F.);
#3291=ADVANCED_FACE('',(#171),#116,.F.);
#3292=ADVANCED_FACE('',(#172),#3161,.F.);
#3293=ADVANCED_FACE('',(#173),#117,.F.);
#3294=ADVANCED_FACE('',(#174),#3162,.T.);
#3295=ADVANCED_FACE('',(#175),#118,.F.);
#3296=ADVANCED_FACE('',(#176),#3163,.T.);
#3297=ADVANCED_FACE('',(#177),#3164,.F.);
#3298=ADVANCED_FACE('',(#178),#3165,.F.);
#3299=ADVANCED_FACE('',(#179),#3166,.T.);
#3300=ADVANCED_FACE('',(#180),#3167,.F.);
#3301=ADVANCED_FACE('',(#181),#119,.F.);
#3302=ADVANCED_FACE('',(#182),#3168,.T.);
#3303=ADVANCED_FACE('',(#183),#3169,.T.);
#3304=ADVANCED_FACE('',(#184),#120,.F.);
#3305=ADVANCED_FACE('',(#185),#121,.T.);
#3306=ADVANCED_FACE('',(#186),#3170,.T.);
#3307=ADVANCED_FACE('',(#187),#3171,.F.);
#3308=ADVANCED_FACE('',(#188),#3172,.F.);
#3309=ADVANCED_FACE('',(#189),#3173,.F.);
#3310=ADVANCED_FACE('',(#190),#3174,.F.);
#3311=ADVANCED_FACE('',(#191,#75,#76),#3175,.F.);
#3312=ADVANCED_FACE('',(#192),#122,.T.);
#3313=ADVANCED_FACE('',(#193),#3176,.F.);
#3314=ADVANCED_FACE('',(#194,#77),#3177,.F.);
#3315=ADVANCED_FACE('',(#195),#3178,.F.);
#3316=ADVANCED_FACE('',(#196),#3179,.T.);
#3317=ADVANCED_FACE('',(#197),#123,.F.);
#3318=ADVANCED_FACE('',(#198),#3180,.T.);
#3319=ADVANCED_FACE('',(#199),#124,.F.);
#3320=ADVANCED_FACE('',(#200),#3181,.T.);
#3321=ADVANCED_FACE('',(#201),#125,.T.);
#3322=ADVANCED_FACE('',(#202),#3182,.T.);
#3323=ADVANCED_FACE('',(#203),#126,.F.);
#3324=ADVANCED_FACE('',(#204),#3183,.T.);
#3325=ADVANCED_FACE('',(#205),#127,.T.);
#3326=ADVANCED_FACE('',(#206),#128,.T.);
#3327=ADVANCED_FACE('',(#207),#3184,.T.);
#3328=ADVANCED_FACE('',(#208),#129,.F.);
#3329=ADVANCED_FACE('',(#209),#3185,.T.);
#3330=ADVANCED_FACE('',(#210),#130,.T.);
#3331=ADVANCED_FACE('',(#211),#3186,.T.);
#3332=ADVANCED_FACE('',(#212),#131,.F.);
#3333=ADVANCED_FACE('',(#213),#132,.T.);
#3334=ADVANCED_FACE('',(#214),#3187,.F.);
#3335=ADVANCED_FACE('',(#215),#3188,.F.);
#3336=ADVANCED_FACE('',(#216),#3189,.T.);
#3337=ADVANCED_FACE('',(#217),#3190,.T.);
#3338=ADVANCED_FACE('',(#218),#3191,.T.);
#3339=ADVANCED_FACE('',(#219),#133,.T.);
#3340=ADVANCED_FACE('',(#220),#3192,.T.);
#3341=ADVANCED_FACE('',(#221),#134,.T.);
#3342=ADVANCED_FACE('',(#222),#3193,.T.);
#3343=ADVANCED_FACE('',(#223),#135,.F.);
#3344=ADVANCED_FACE('',(#224),#3194,.T.);
#3345=ADVANCED_FACE('',(#225),#3195,.F.);
#3346=ADVANCED_FACE('',(#226),#136,.F.);
#3347=ADVANCED_FACE('',(#227),#3196,.F.);
#3348=ADVANCED_FACE('',(#228),#3197,.F.);
#3349=ADVANCED_FACE('',(#229),#3198,.F.);
#3350=ADVANCED_FACE('',(#230),#3199,.F.);
#3351=ADVANCED_FACE('',(#231),#3200,.F.);
#3352=ADVANCED_FACE('',(#232),#3201,.T.);
#3353=ADVANCED_FACE('',(#233,#78),#3202,.T.);
#3354=ADVANCED_FACE('',(#234,#79),#3203,.T.);
#3355=ADVANCED_FACE('',(#235),#3204,.T.);
#3356=ADVANCED_FACE('',(#236),#3205,.T.);
#3357=ADVANCED_FACE('',(#237),#3206,.T.);
#3358=ADVANCED_FACE('',(#238),#3207,.T.);
#3359=ADVANCED_FACE('',(#239,#80,#81),#3208,.T.);
#3360=ADVANCED_FACE('',(#240),#137,.F.);
#3361=ADVANCED_FACE('',(#241),#3209,.T.);
#3362=ADVANCED_FACE('',(#242,#82),#3210,.T.);
#3363=ADVANCED_FACE('',(#243),#3211,.T.);
#3364=ADVANCED_FACE('',(#244),#3212,.T.);
#3365=ADVANCED_FACE('',(#245),#3213,.T.);
#3366=ADVANCED_FACE('',(#246,#83),#3214,.T.);
#3367=ADVANCED_FACE('',(#247),#3215,.F.);
#3368=ADVANCED_FACE('',(#248),#3216,.F.);
#3369=ADVANCED_FACE('',(#249,#84,#85),#3217,.F.);
#3370=ADVANCED_FACE('',(#250),#3218,.T.);
#3371=ADVANCED_FACE('',(#251),#138,.F.);
#3372=ADVANCED_FACE('',(#252),#139,.F.);
#3373=ADVANCED_FACE('',(#253),#3219,.T.);
#3374=ADVANCED_FACE('',(#254),#3220,.T.);
#3375=ADVANCED_FACE('',(#255),#140,.F.);
#3376=ADVANCED_FACE('',(#256),#141,.F.);
#3377=ADVANCED_FACE('',(#257),#3221,.T.);
#3378=ADVANCED_FACE('',(#258),#142,.F.);
#3379=ADVANCED_FACE('',(#259),#3222,.T.);
#3380=ADVANCED_FACE('',(#260),#3223,.T.);
#3381=ADVANCED_FACE('',(#261),#143,.T.);
#3382=ADVANCED_FACE('',(#262),#144,.F.);
#3383=ADVANCED_FACE('',(#263),#3224,.T.);
#3384=ADVANCED_FACE('',(#264),#145,.F.);
#3385=ADVANCED_FACE('',(#265),#3225,.F.);
#3386=ADVANCED_FACE('',(#266),#3226,.F.);
#3387=ADVANCED_FACE('',(#267),#3227,.F.);
#3388=ADVANCED_FACE('',(#268),#3228,.T.);
#3389=ADVANCED_FACE('',(#269),#3229,.T.);
#3390=ADVANCED_FACE('',(#270),#146,.T.);
#3391=ADVANCED_FACE('',(#271),#147,.F.);
#3392=ADVANCED_FACE('',(#272),#3230,.T.);
#3393=ADVANCED_FACE('',(#273),#148,.T.);
#3394=ADVANCED_FACE('',(#274),#149,.F.);
#3395=ADVANCED_FACE('',(#275),#3231,.T.);
#3396=ADVANCED_FACE('',(#276),#150,.F.);
#3397=ADVANCED_FACE('',(#277),#3232,.T.);
#3398=ADVANCED_FACE('',(#278),#151,.T.);
#3399=ADVANCED_FACE('',(#279,#86,#87),#3233,.F.);
#3400=ADVANCED_FACE('',(#280),#3234,.F.);
#3401=ADVANCED_FACE('',(#281),#3235,.F.);
#3402=ADVANCED_FACE('',(#282),#3236,.F.);
#3403=ADVANCED_FACE('',(#283),#3237,.T.);
#3404=ADVANCED_FACE('',(#284),#3238,.F.);
#3405=ADVANCED_FACE('',(#285),#3239,.T.);
#3406=ADVANCED_FACE('',(#286),#3240,.T.);
#3407=ADVANCED_FACE('',(#287),#3241,.T.);
#3408=ADVANCED_FACE('',(#288),#3242,.T.);
#3409=ADVANCED_FACE('',(#289,#88),#3243,.T.);
#3410=ADVANCED_FACE('',(#290),#152,.T.);
#3411=ADVANCED_FACE('',(#291),#3244,.T.);
#3412=ADVANCED_FACE('',(#292,#89),#3245,.T.);
#3413=ADVANCED_FACE('',(#293),#3246,.T.);
#3414=ADVANCED_FACE('',(#294),#3247,.T.);
#3415=ADVANCED_FACE('',(#295),#3248,.T.);
#3416=ADVANCED_FACE('',(#296),#3249,.F.);
#3417=ADVANCED_FACE('',(#297),#3250,.F.);
#3418=ADVANCED_FACE('',(#298),#3251,.F.);
#3419=ADVANCED_FACE('',(#299),#3252,.F.);
#3420=ADVANCED_FACE('',(#300),#3253,.T.);
#3421=ADVANCED_FACE('',(#301),#3254,.F.);
#3422=ADVANCED_FACE('',(#302),#153,.F.);
#3423=ADVANCED_FACE('',(#303),#3255,.T.);
#3424=ADVANCED_FACE('',(#304),#3256,.T.);
#3425=ADVANCED_FACE('',(#305),#154,.F.);
#3426=ADVANCED_FACE('',(#306),#155,.T.);
#3427=ADVANCED_FACE('',(#307),#3257,.T.);
#3428=ADVANCED_FACE('',(#308),#3258,.F.);
#3429=ADVANCED_FACE('',(#309),#3259,.F.);
#3430=ADVANCED_FACE('',(#310),#3260,.F.);
#3431=ADVANCED_FACE('',(#311),#3261,.F.);
#3432=ADVANCED_FACE('',(#312,#90,#91),#3262,.T.);
#3433=ADVANCED_FACE('',(#313,#92),#3263,.F.);
#3434=ADVANCED_FACE('',(#314,#93,#94),#3264,.F.);
#3435=ADVANCED_FACE('',(#315),#3265,.T.);
#3436=ADVANCED_FACE('',(#316),#156,.T.);
#3437=ADVANCED_FACE('',(#317),#3266,.F.);
#3438=ADVANCED_FACE('',(#318),#3267,.F.);
#3439=ADVANCED_FACE('',(#319,#95),#3268,.F.);
#3440=ADVANCED_FACE('',(#320),#3269,.F.);
#3441=ADVANCED_FACE('',(#321),#3270,.T.);
#3442=ADVANCED_FACE('',(#322),#157,.F.);
#3443=ADVANCED_FACE('',(#323),#3271,.T.);
#3444=ADVANCED_FACE('',(#324),#158,.F.);
#3445=ADVANCED_FACE('',(#325),#3272,.T.);
#3446=ADVANCED_FACE('',(#326),#159,.T.);
#3447=ADVANCED_FACE('',(#327),#3273,.T.);
#3448=ADVANCED_FACE('',(#328),#160,.F.);
#3449=ADVANCED_FACE('',(#329),#3274,.T.);
#3450=ADVANCED_FACE('',(#330),#161,.T.);
#3451=ADVANCED_FACE('',(#331),#3275,.T.);
#3452=ADVANCED_FACE('',(#332),#3276,.F.);
#3453=ADVANCED_FACE('',(#333),#162,.T.);
#3454=ADVANCED_FACE('',(#334),#3277,.T.);
#3455=ADVANCED_FACE('',(#335),#163,.T.);
#3456=ADVANCED_FACE('',(#336),#3278,.T.);
#3457=ADVANCED_FACE('',(#337),#3279,.F.);
#3458=ADVANCED_FACE('',(#338),#164,.T.);
#3459=ADVANCED_FACE('',(#339),#3280,.T.);
#3460=ADVANCED_FACE('',(#340),#3281,.F.);
#3461=ADVANCED_FACE('',(#341),#165,.T.);
#3462=ADVANCED_FACE('',(#342),#3282,.T.);
#3463=ADVANCED_FACE('',(#343),#3283,.F.);
#3464=ADVANCED_FACE('',(#344),#3284,.F.);
#3465=ADVANCED_FACE('',(#345),#166,.T.);
#3466=ADVANCED_FACE('',(#346),#3285,.T.);
#3467=ADVANCED_FACE('',(#347),#167,.T.);
#3468=ADVANCED_FACE('',(#348),#3286,.F.);
#3469=ADVANCED_FACE('',(#349),#3287,.T.);
#3470=CLOSED_SHELL('',(#3288,#3289,#3290,#3291,#3292,#3293,#3294,#3295,
#3296,#3297,#3298,#3299,#3300,#3301,#3302,#3303,#3304,#3305,#3306,#3307,
#3308,#3309,#3310,#3311,#3312,#3313,#3314,#3315,#3316,#3317,#3318,#3319,
#3320,#3321,#3322,#3323,#3324,#3325,#3326,#3327,#3328,#3329,#3330,#3331,
#3332,#3333,#3334,#3335,#3336,#3337,#3338,#3339,#3340,#3341,#3342,#3343,
#3344,#3345,#3346,#3347,#3348,#3349,#3350,#3351,#3352,#3353,#3354,#3355,
#3356,#3357,#3358,#3359,#3360,#3361,#3362,#3363,#3364,#3365,#3366,#3367,
#3368,#3369));
#3471=CLOSED_SHELL('',(#3370,#3371,#3372,#3373,#3374,#3375,#3376,#3377,
#3378,#3379,#3380,#3381,#3382,#3383,#3384,#3385,#3386,#3387,#3388,#3389,
#3390,#3391,#3392,#3393,#3394,#3395,#3396,#3397,#3398,#3399,#3400,#3401,
#3402,#3403,#3404,#3405,#3406,#3407,#3408,#3409,#3410,#3411,#3412,#3413,
#3414,#3415,#3416,#3417,#3418,#3419,#3420,#3421,#3422,#3423,#3424,#3425,
#3426,#3427,#3428,#3429,#3430,#3431,#3432,#3433,#3434,#3435,#3436,#3437,
#3438,#3439,#3440,#3441,#3442,#3443,#3444,#3445,#3446,#3447,#3448,#3449,
#3450,#3451));
#3472=CLOSED_SHELL('',(#3452,#3453,#3454));
#3473=CLOSED_SHELL('',(#3455,#3456,#3457));
#3474=CLOSED_SHELL('',(#3458,#3459,#3460));
#3475=CLOSED_SHELL('',(#3461,#3462,#3463));
#3476=CLOSED_SHELL('',(#3464,#3465,#3466));
#3477=CLOSED_SHELL('',(#3467,#3468,#3469));
#3478=DERIVED_UNIT_ELEMENT(#3494,1.);
#3479=DERIVED_UNIT_ELEMENT(#5914,-3.);
#3480=DERIVED_UNIT_ELEMENT(#3494,1.);
#3481=DERIVED_UNIT_ELEMENT(#5914,-3.);
#3482=DERIVED_UNIT_ELEMENT(#3494,1.);
#3483=DERIVED_UNIT_ELEMENT(#5914,-3.);
#3484=DERIVED_UNIT_ELEMENT(#3494,1.);
#3485=DERIVED_UNIT_ELEMENT(#5914,-3.);
#3486=DERIVED_UNIT_ELEMENT(#3494,1.);
#3487=DERIVED_UNIT_ELEMENT(#5914,-3.);
#3488=DERIVED_UNIT_ELEMENT(#3494,1.);
#3489=DERIVED_UNIT_ELEMENT(#5914,-3.);
#3490=DERIVED_UNIT_ELEMENT(#3494,1.);
#3491=DERIVED_UNIT_ELEMENT(#5914,-3.);
#3492=DERIVED_UNIT_ELEMENT(#3494,1.);
#3493=DERIVED_UNIT_ELEMENT(#5914,-3.);
#3494=(
MASS_UNIT()
NAMED_UNIT(*)
SI_UNIT(.KILO.,.GRAM.)
);
#3495=DERIVED_UNIT((#3478,#3479));
#3496=DERIVED_UNIT((#3480,#3481));
#3497=DERIVED_UNIT((#3482,#3483));
#3498=DERIVED_UNIT((#3484,#3485));
#3499=DERIVED_UNIT((#3486,#3487));
#3500=DERIVED_UNIT((#3488,#3489));
#3501=DERIVED_UNIT((#3490,#3491));
#3502=DERIVED_UNIT((#3492,#3493));
#3503=MEASURE_REPRESENTATION_ITEM('density measure',
POSITIVE_RATIO_MEASURE(7850.),#3495);
#3504=MEASURE_REPRESENTATION_ITEM('density measure',
POSITIVE_RATIO_MEASURE(7850.),#3496);
#3505=MEASURE_REPRESENTATION_ITEM('density measure',
POSITIVE_RATIO_MEASURE(7850.),#3497);
#3506=MEASURE_REPRESENTATION_ITEM('density measure',
POSITIVE_RATIO_MEASURE(7850.),#3498);
#3507=MEASURE_REPRESENTATION_ITEM('density measure',
POSITIVE_RATIO_MEASURE(7850.),#3499);
#3508=MEASURE_REPRESENTATION_ITEM('density measure',
POSITIVE_RATIO_MEASURE(7850.),#3500);
#3509=MEASURE_REPRESENTATION_ITEM('density measure',
POSITIVE_RATIO_MEASURE(7850.),#3501);
#3510=MEASURE_REPRESENTATION_ITEM('density measure',
POSITIVE_RATIO_MEASURE(7850.),#3502);
#3511=PROPERTY_DEFINITION_REPRESENTATION(#3551,#3527);
#3512=PROPERTY_DEFINITION_REPRESENTATION(#3552,#3528);
#3513=PROPERTY_DEFINITION_REPRESENTATION(#3553,#3529);
#3514=PROPERTY_DEFINITION_REPRESENTATION(#3554,#3530);
#3515=PROPERTY_DEFINITION_REPRESENTATION(#3555,#3531);
#3516=PROPERTY_DEFINITION_REPRESENTATION(#3556,#3532);
#3517=PROPERTY_DEFINITION_REPRESENTATION(#3557,#3533);
#3518=PROPERTY_DEFINITION_REPRESENTATION(#3558,#3534);
#3519=PROPERTY_DEFINITION_REPRESENTATION(#3559,#3535);
#3520=PROPERTY_DEFINITION_REPRESENTATION(#3560,#3536);
#3521=PROPERTY_DEFINITION_REPRESENTATION(#3561,#3537);
#3522=PROPERTY_DEFINITION_REPRESENTATION(#3562,#3538);
#3523=PROPERTY_DEFINITION_REPRESENTATION(#3563,#3539);
#3524=PROPERTY_DEFINITION_REPRESENTATION(#3564,#3540);
#3525=PROPERTY_DEFINITION_REPRESENTATION(#3565,#3541);
#3526=PROPERTY_DEFINITION_REPRESENTATION(#3566,#3542);
#3527=REPRESENTATION('material name',(#3543),#5904);
#3528=REPRESENTATION('density',(#3503),#5904);
#3529=REPRESENTATION('material name',(#3544),#5905);
#3530=REPRESENTATION('density',(#3504),#5905);
#3531=REPRESENTATION('material name',(#3545),#5906);
#3532=REPRESENTATION('density',(#3505),#5906);
#3533=REPRESENTATION('material name',(#3546),#5907);
#3534=REPRESENTATION('density',(#3506),#5907);
#3535=REPRESENTATION('material name',(#3547),#5908);
#3536=REPRESENTATION('density',(#3507),#5908);
#3537=REPRESENTATION('material name',(#3548),#5909);
#3538=REPRESENTATION('density',(#3508),#5909);
#3539=REPRESENTATION('material name',(#3549),#5910);
#3540=REPRESENTATION('density',(#3509),#5910);
#3541=REPRESENTATION('material name',(#3550),#5911);
#3542=REPRESENTATION('density',(#3510),#5911);
#3543=DESCRIPTIVE_REPRESENTATION_ITEM('Steel','Steel');
#3544=DESCRIPTIVE_REPRESENTATION_ITEM('Steel','Steel');
#3545=DESCRIPTIVE_REPRESENTATION_ITEM('Steel','Steel');
#3546=DESCRIPTIVE_REPRESENTATION_ITEM('Steel','Steel');
#3547=DESCRIPTIVE_REPRESENTATION_ITEM('Steel','Steel');
#3548=DESCRIPTIVE_REPRESENTATION_ITEM('Steel','Steel');
#3549=DESCRIPTIVE_REPRESENTATION_ITEM('Steel','Steel');
#3550=DESCRIPTIVE_REPRESENTATION_ITEM('Steel','Steel');
#3551=PROPERTY_DEFINITION('material property','material name',#5954);
#3552=PROPERTY_DEFINITION('material property','density of part',#5954);
#3553=PROPERTY_DEFINITION('material property','material name',#5955);
#3554=PROPERTY_DEFINITION('material property','density of part',#5955);
#3555=PROPERTY_DEFINITION('material property','material name',#5956);
#3556=PROPERTY_DEFINITION('material property','density of part',#5956);
#3557=PROPERTY_DEFINITION('material property','material name',#5957);
#3558=PROPERTY_DEFINITION('material property','density of part',#5957);
#3559=PROPERTY_DEFINITION('material property','material name',#5958);
#3560=PROPERTY_DEFINITION('material property','density of part',#5958);
#3561=PROPERTY_DEFINITION('material property','material name',#5959);
#3562=PROPERTY_DEFINITION('material property','density of part',#5959);
#3563=PROPERTY_DEFINITION('material property','material name',#5960);
#3564=PROPERTY_DEFINITION('material property','density of part',#5960);
#3565=PROPERTY_DEFINITION('material property','material name',#5961);
#3566=PROPERTY_DEFINITION('material property','density of part',#5961);
#3567=AXIS2_PLACEMENT_3D('',#4889,#3886,#3887);
#3568=AXIS2_PLACEMENT_3D('',#4890,#3888,#3889);
#3569=AXIS2_PLACEMENT_3D('',#4891,#3890,#3891);
#3570=AXIS2_PLACEMENT_3D('',#4895,#3893,#3894);
#3571=AXIS2_PLACEMENT_3D('',#4896,#3895,#3896);
#3572=AXIS2_PLACEMENT_3D('',#4898,#3897,#3898);
#3573=AXIS2_PLACEMENT_3D('',#4901,#3900,#3901);
#3574=AXIS2_PLACEMENT_3D('',#4902,#3902,#3903);
#3575=AXIS2_PLACEMENT_3D('',#4903,#3904,#3905);
#3576=AXIS2_PLACEMENT_3D('',#4905,#3906,#3907);
#3577=AXIS2_PLACEMENT_3D('',#4908,#3909,#3910);
#3578=AXIS2_PLACEMENT_3D('',#4909,#3911,#3912);
#3579=AXIS2_PLACEMENT_3D('',#4912,#3913,#3914);
#3580=AXIS2_PLACEMENT_3D('',#4914,#3915,#3916);
#3581=AXIS2_PLACEMENT_3D('',#4915,#3917,#3918);
#3582=AXIS2_PLACEMENT_3D('',#4918,#3920,#3921);
#3583=AXIS2_PLACEMENT_3D('',#4919,#3922,#3923);
#3584=AXIS2_PLACEMENT_3D('',#4929,#3929,#3930);
#3585=AXIS2_PLACEMENT_3D('',#4931,#3931,#3932);
#3586=AXIS2_PLACEMENT_3D('',#4934,#3934,#3935);
#3587=AXIS2_PLACEMENT_3D('',#4935,#3936,#3937);
#3588=AXIS2_PLACEMENT_3D('',#4936,#3938,#3939);
#3589=AXIS2_PLACEMENT_3D('',#4938,#3940,#3941);
#3590=AXIS2_PLACEMENT_3D('',#4941,#3943,#3944);
#3591=AXIS2_PLACEMENT_3D('',#4942,#3945,#3946);
#3592=AXIS2_PLACEMENT_3D('',#4943,#3947,#3948);
#3593=AXIS2_PLACEMENT_3D('',#4953,#3954,#3955);
#3594=AXIS2_PLACEMENT_3D('',#4966,#3962,#3963);
#3595=AXIS2_PLACEMENT_3D('',#4974,#3968,#3969);
#3596=AXIS2_PLACEMENT_3D('',#4976,#3970,#3971);
#3597=AXIS2_PLACEMENT_3D('',#4977,#3972,#3973);
#3598=AXIS2_PLACEMENT_3D('',#4980,#3975,#3976);
#3599=AXIS2_PLACEMENT_3D('',#4981,#3977,#3978);
#3600=AXIS2_PLACEMENT_3D('',#4991,#3984,#3985);
#3601=AXIS2_PLACEMENT_3D('',#5000,#3990,#3991);
#3602=AXIS2_PLACEMENT_3D('',#5001,#3992,#3993);
#3603=AXIS2_PLACEMENT_3D('',#5002,#3994,#3995);
#3604=AXIS2_PLACEMENT_3D('',#5003,#3996,#3997);
#3605=AXIS2_PLACEMENT_3D('',#5005,#3998,#3999);
#3606=AXIS2_PLACEMENT_3D('',#5006,#4000,#4001);
#3607=AXIS2_PLACEMENT_3D('',#5008,#4003,#4004);
#3608=AXIS2_PLACEMENT_3D('',#5014,#4008,#4009);
#3609=AXIS2_PLACEMENT_3D('',#5020,#4013,#4014);
#3610=AXIS2_PLACEMENT_3D('',#5024,#4017,#4018);
#3611=AXIS2_PLACEMENT_3D('',#5028,#4021,#4022);
#3612=AXIS2_PLACEMENT_3D('',#5032,#4025,#4026);
#3613=AXIS2_PLACEMENT_3D('',#5040,#4030,#4031);
#3614=AXIS2_PLACEMENT_3D('',#5044,#4034,#4035);
#3615=AXIS2_PLACEMENT_3D('',#5046,#4036,#4037);
#3616=AXIS2_PLACEMENT_3D('',#5049,#4039,#4040);
#3617=AXIS2_PLACEMENT_3D('',#5050,#4041,#4042);
#3618=AXIS2_PLACEMENT_3D('',#5054,#4045,#4046);
#3619=AXIS2_PLACEMENT_3D('',#5056,#4048,#4049);
#3620=AXIS2_PLACEMENT_3D('',#5060,#4052,#4053);
#3621=AXIS2_PLACEMENT_3D('',#5068,#4058,#4059);
#3622=AXIS2_PLACEMENT_3D('',#5070,#4060,#4061);
#3623=AXIS2_PLACEMENT_3D('',#5072,#4062,#4063);
#3624=AXIS2_PLACEMENT_3D('',#5074,#4065,#4066);
#3625=AXIS2_PLACEMENT_3D('',#5080,#4070,#4071);
#3626=AXIS2_PLACEMENT_3D('',#5081,#4072,#4073);
#3627=AXIS2_PLACEMENT_3D('',#5082,#4074,#4075);
#3628=AXIS2_PLACEMENT_3D('',#5083,#4076,#4077);
#3629=AXIS2_PLACEMENT_3D('',#5089,#4081,#4082);
#3630=AXIS2_PLACEMENT_3D('',#5091,#4083,#4084);
#3631=AXIS2_PLACEMENT_3D('',#5093,#4085,#4086);
#3632=AXIS2_PLACEMENT_3D('',#5095,#4088,#4089);
#3633=AXIS2_PLACEMENT_3D('',#5101,#4093,#4094);
#3634=AXIS2_PLACEMENT_3D('',#5103,#4095,#4096);
#3635=AXIS2_PLACEMENT_3D('',#5105,#4097,#4098);
#3636=AXIS2_PLACEMENT_3D('',#5107,#4100,#4101);
#3637=AXIS2_PLACEMENT_3D('',#5113,#4105,#4106);
#3638=AXIS2_PLACEMENT_3D('',#5115,#4107,#4108);
#3639=AXIS2_PLACEMENT_3D('',#5118,#4110,#4111);
#3640=AXIS2_PLACEMENT_3D('',#5119,#4112,#4113);
#3641=AXIS2_PLACEMENT_3D('',#5122,#4114,#4115);
#3642=AXIS2_PLACEMENT_3D('',#5126,#4117,#4118);
#3643=AXIS2_PLACEMENT_3D('',#5128,#4119,#4120);
#3644=AXIS2_PLACEMENT_3D('',#5130,#4122,#4123);
#3645=AXIS2_PLACEMENT_3D('',#5136,#4127,#4128);
#3646=AXIS2_PLACEMENT_3D('',#5138,#4129,#4130);
#3647=AXIS2_PLACEMENT_3D('',#5141,#4132,#4133);
#3648=AXIS2_PLACEMENT_3D('',#5142,#4134,#4135);
#3649=AXIS2_PLACEMENT_3D('',#5148,#4139,#4140);
#3650=AXIS2_PLACEMENT_3D('',#5150,#4141,#4142);
#3651=AXIS2_PLACEMENT_3D('',#5153,#4144,#4145);
#3652=AXIS2_PLACEMENT_3D('',#5154,#4146,#4147);
#3653=AXIS2_PLACEMENT_3D('',#5163,#4152,#4153);
#3654=AXIS2_PLACEMENT_3D('',#5165,#4154,#4155);
#3655=AXIS2_PLACEMENT_3D('',#5168,#4157,#4158);
#3656=AXIS2_PLACEMENT_3D('',#5169,#4159,#4160);
#3657=AXIS2_PLACEMENT_3D('',#5173,#4162,#4163);
#3658=AXIS2_PLACEMENT_3D('',#5175,#4165,#4166);
#3659=AXIS2_PLACEMENT_3D('',#5184,#4171,#4172);
#3660=AXIS2_PLACEMENT_3D('',#5193,#4177,#4178);
#3661=AXIS2_PLACEMENT_3D('',#5206,#4185,#4186);
#3662=AXIS2_PLACEMENT_3D('',#5219,#4193,#4194);
#3663=AXIS2_PLACEMENT_3D('',#5222,#4197,#4198);
#3664=AXIS2_PLACEMENT_3D('',#5224,#4199,#4200);
#3665=AXIS2_PLACEMENT_3D('',#5227,#4202,#4203);
#3666=AXIS2_PLACEMENT_3D('',#5228,#4204,#4205);
#3667=AXIS2_PLACEMENT_3D('',#5234,#4209,#4210);
#3668=AXIS2_PLACEMENT_3D('',#5236,#4211,#4212);
#3669=AXIS2_PLACEMENT_3D('',#5240,#4214,#4215);
#3670=AXIS2_PLACEMENT_3D('',#5242,#4217,#4218);
#3671=AXIS2_PLACEMENT_3D('',#5253,#4226,#4227);
#3672=AXIS2_PLACEMENT_3D('',#5256,#4228,#4229);
#3673=AXIS2_PLACEMENT_3D('',#5260,#4231,#4232);
#3674=AXIS2_PLACEMENT_3D('',#5262,#4234,#4235);
#3675=AXIS2_PLACEMENT_3D('',#5268,#4239,#4240);
#3676=AXIS2_PLACEMENT_3D('',#5270,#4242,#4243);
#3677=AXIS2_PLACEMENT_3D('',#5272,#4245,#4246);
#3678=AXIS2_PLACEMENT_3D('',#5274,#4247,#4248);
#3679=AXIS2_PLACEMENT_3D('',#5277,#4250,#4251);
#3680=AXIS2_PLACEMENT_3D('',#5278,#4252,#4253);
#3681=AXIS2_PLACEMENT_3D('',#5279,#4254,#4255);
#3682=AXIS2_PLACEMENT_3D('',#5288,#4260,#4261);
#3683=AXIS2_PLACEMENT_3D('',#5295,#4266,#4267);
#3684=AXIS2_PLACEMENT_3D('',#5299,#4270,#4271);
#3685=AXIS2_PLACEMENT_3D('',#5301,#4273,#4274);
#3686=AXIS2_PLACEMENT_3D('',#5307,#4278,#4279);
#3687=AXIS2_PLACEMENT_3D('',#5309,#4281,#4282);
#3688=AXIS2_PLACEMENT_3D('',#5313,#4285,#4286);
#3689=AXIS2_PLACEMENT_3D('',#5317,#4289,#4290);
#3690=AXIS2_PLACEMENT_3D('',#5319,#4292,#4293);
#3691=AXIS2_PLACEMENT_3D('',#5320,#4294,#4295);
#3692=AXIS2_PLACEMENT_3D('',#5333,#4302,#4303);
#3693=AXIS2_PLACEMENT_3D('',#5334,#4304,#4305);
#3694=AXIS2_PLACEMENT_3D('',#5336,#4307,#4308);
#3695=AXIS2_PLACEMENT_3D('',#5337,#4309,#4310);
#3696=AXIS2_PLACEMENT_3D('',#5343,#4316,#4317);
#3697=AXIS2_PLACEMENT_3D('',#5345,#4319,#4320);
#3698=AXIS2_PLACEMENT_3D('',#5347,#4322,#4323);
#3699=AXIS2_PLACEMENT_3D('',#5349,#4325,#4326);
#3700=AXIS2_PLACEMENT_3D('',#5351,#4328,#4329);
#3701=AXIS2_PLACEMENT_3D('',#5353,#4331,#4332);
#3702=AXIS2_PLACEMENT_3D('',#5355,#4334,#4335);
#3703=AXIS2_PLACEMENT_3D('',#5357,#4337,#4338);
#3704=AXIS2_PLACEMENT_3D('',#5358,#4339,#4340);
#3705=AXIS2_PLACEMENT_3D('',#5359,#4341,#4342);
#3706=AXIS2_PLACEMENT_3D('',#5363,#4344,#4345);
#3707=AXIS2_PLACEMENT_3D('',#5364,#4346,#4347);
#3708=AXIS2_PLACEMENT_3D('',#5367,#4348,#4349);
#3709=AXIS2_PLACEMENT_3D('',#5369,#4350,#4351);
#3710=AXIS2_PLACEMENT_3D('',#5370,#4352,#4353);
#3711=AXIS2_PLACEMENT_3D('',#5373,#4355,#4356);
#3712=AXIS2_PLACEMENT_3D('',#5374,#4357,#4358);
#3713=AXIS2_PLACEMENT_3D('',#5375,#4359,#4360);
#3714=AXIS2_PLACEMENT_3D('',#5377,#4361,#4362);
#3715=AXIS2_PLACEMENT_3D('',#5381,#4364,#4365);
#3716=AXIS2_PLACEMENT_3D('',#5383,#4366,#4367);
#3717=AXIS2_PLACEMENT_3D('',#5384,#4368,#4369);
#3718=AXIS2_PLACEMENT_3D('',#5385,#4370,#4371);
#3719=AXIS2_PLACEMENT_3D('',#5395,#4377,#4378);
#3720=AXIS2_PLACEMENT_3D('',#5405,#4384,#4385);
#3721=AXIS2_PLACEMENT_3D('',#5407,#4386,#4387);
#3722=AXIS2_PLACEMENT_3D('',#5410,#4389,#4390);
#3723=AXIS2_PLACEMENT_3D('',#5411,#4391,#4392);
#3724=AXIS2_PLACEMENT_3D('',#5413,#4393,#4394);
#3725=AXIS2_PLACEMENT_3D('',#5416,#4396,#4397);
#3726=AXIS2_PLACEMENT_3D('',#5417,#4398,#4399);
#3727=AXIS2_PLACEMENT_3D('',#5418,#4400,#4401);
#3728=AXIS2_PLACEMENT_3D('',#5420,#4402,#4403);
#3729=AXIS2_PLACEMENT_3D('',#5423,#4405,#4406);
#3730=AXIS2_PLACEMENT_3D('',#5424,#4407,#4408);
#3731=AXIS2_PLACEMENT_3D('',#5425,#4409,#4410);
#3732=AXIS2_PLACEMENT_3D('',#5434,#4415,#4416);
#3733=AXIS2_PLACEMENT_3D('',#5436,#4417,#4418);
#3734=AXIS2_PLACEMENT_3D('',#5440,#4420,#4421);
#3735=AXIS2_PLACEMENT_3D('',#5442,#4423,#4424);
#3736=AXIS2_PLACEMENT_3D('',#5445,#4425,#4426);
#3737=AXIS2_PLACEMENT_3D('',#5449,#4428,#4429);
#3738=AXIS2_PLACEMENT_3D('',#5451,#4431,#4432);
#3739=AXIS2_PLACEMENT_3D('',#5457,#4436,#4437);
#3740=AXIS2_PLACEMENT_3D('',#5459,#4438,#4439);
#3741=AXIS2_PLACEMENT_3D('',#5462,#4441,#4442);
#3742=AXIS2_PLACEMENT_3D('',#5463,#4443,#4444);
#3743=AXIS2_PLACEMENT_3D('',#5464,#4445,#4446);
#3744=AXIS2_PLACEMENT_3D('',#5473,#4451,#4452);
#3745=AXIS2_PLACEMENT_3D('',#5482,#4457,#4458);
#3746=AXIS2_PLACEMENT_3D('',#5492,#4464,#4465);
#3747=AXIS2_PLACEMENT_3D('',#5502,#4471,#4472);
#3748=AXIS2_PLACEMENT_3D('',#5505,#4473,#4474);
#3749=AXIS2_PLACEMENT_3D('',#5509,#4476,#4477);
#3750=AXIS2_PLACEMENT_3D('',#5511,#4478,#4479);
#3751=AXIS2_PLACEMENT_3D('',#5513,#4481,#4482);
#3752=AXIS2_PLACEMENT_3D('',#5516,#4483,#4484);
#3753=AXIS2_PLACEMENT_3D('',#5520,#4486,#4487);
#3754=AXIS2_PLACEMENT_3D('',#5522,#4489,#4490);
#3755=AXIS2_PLACEMENT_3D('',#5528,#4494,#4495);
#3756=AXIS2_PLACEMENT_3D('',#5530,#4496,#4497);
#3757=AXIS2_PLACEMENT_3D('',#5533,#4499,#4500);
#3758=AXIS2_PLACEMENT_3D('',#5534,#4501,#4502);
#3759=AXIS2_PLACEMENT_3D('',#5536,#4503,#4504);
#3760=AXIS2_PLACEMENT_3D('',#5539,#4506,#4507);
#3761=AXIS2_PLACEMENT_3D('',#5540,#4508,#4509);
#3762=AXIS2_PLACEMENT_3D('',#5546,#4513,#4514);
#3763=AXIS2_PLACEMENT_3D('',#5548,#4515,#4516);
#3764=AXIS2_PLACEMENT_3D('',#5551,#4518,#4519);
#3765=AXIS2_PLACEMENT_3D('',#5552,#4520,#4521);
#3766=AXIS2_PLACEMENT_3D('',#5567,#4532,#4533);
#3767=AXIS2_PLACEMENT_3D('',#5569,#4534,#4535);
#3768=AXIS2_PLACEMENT_3D('',#5571,#4537,#4538);
#3769=AXIS2_PLACEMENT_3D('',#5581,#4545,#4546);
#3770=AXIS2_PLACEMENT_3D('',#5585,#4549,#4550);
#3771=AXIS2_PLACEMENT_3D('',#5587,#4552,#4553);
#3772=AXIS2_PLACEMENT_3D('',#5593,#4557,#4558);
#3773=AXIS2_PLACEMENT_3D('',#5603,#4564,#4565);
#3774=AXIS2_PLACEMENT_3D('',#5605,#4567,#4568);
#3775=AXIS2_PLACEMENT_3D('',#5613,#4573,#4574);
#3776=AXIS2_PLACEMENT_3D('',#5616,#4577,#4578);
#3777=AXIS2_PLACEMENT_3D('',#5618,#4580,#4581);
#3778=AXIS2_PLACEMENT_3D('',#5619,#4582,#4583);
#3779=AXIS2_PLACEMENT_3D('',#5620,#4584,#4585);
#3780=AXIS2_PLACEMENT_3D('',#5621,#4586,#4587);
#3781=AXIS2_PLACEMENT_3D('',#5622,#4588,#4589);
#3782=AXIS2_PLACEMENT_3D('',#5623,#4590,#4591);
#3783=AXIS2_PLACEMENT_3D('',#5628,#4596,#4597);
#3784=AXIS2_PLACEMENT_3D('',#5630,#4599,#4600);
#3785=AXIS2_PLACEMENT_3D('',#5632,#4602,#4603);
#3786=AXIS2_PLACEMENT_3D('',#5634,#4605,#4606);
#3787=AXIS2_PLACEMENT_3D('',#5635,#4607,#4608);
#3788=AXIS2_PLACEMENT_3D('',#5637,#4610,#4611);
#3789=AXIS2_PLACEMENT_3D('',#5638,#4612,#4613);
#3790=AXIS2_PLACEMENT_3D('',#5651,#4620,#4621);
#3791=AXIS2_PLACEMENT_3D('',#5664,#4628,#4629);
#3792=AXIS2_PLACEMENT_3D('',#5672,#4634,#4635);
#3793=AXIS2_PLACEMENT_3D('',#5674,#4636,#4637);
#3794=AXIS2_PLACEMENT_3D('',#5675,#4638,#4639);
#3795=AXIS2_PLACEMENT_3D('',#5678,#4641,#4642);
#3796=AXIS2_PLACEMENT_3D('',#5679,#4643,#4644);
#3797=AXIS2_PLACEMENT_3D('',#5689,#4650,#4651);
#3798=AXIS2_PLACEMENT_3D('',#5698,#4656,#4657);
#3799=AXIS2_PLACEMENT_3D('',#5699,#4658,#4659);
#3800=AXIS2_PLACEMENT_3D('',#5700,#4660,#4661);
#3801=AXIS2_PLACEMENT_3D('',#5701,#4662,#4663);
#3802=AXIS2_PLACEMENT_3D('',#5703,#4664,#4665);
#3803=AXIS2_PLACEMENT_3D('',#5704,#4666,#4667);
#3804=AXIS2_PLACEMENT_3D('',#5706,#4669,#4670);
#3805=AXIS2_PLACEMENT_3D('',#5712,#4674,#4675);
#3806=AXIS2_PLACEMENT_3D('',#5718,#4679,#4680);
#3807=AXIS2_PLACEMENT_3D('',#5722,#4683,#4684);
#3808=AXIS2_PLACEMENT_3D('',#5728,#4688,#4689);
#3809=AXIS2_PLACEMENT_3D('',#5732,#4692,#4693);
#3810=AXIS2_PLACEMENT_3D('',#5736,#4695,#4696);
#3811=AXIS2_PLACEMENT_3D('',#5741,#4699,#4700);
#3812=AXIS2_PLACEMENT_3D('',#5745,#4702,#4703);
#3813=AXIS2_PLACEMENT_3D('',#5749,#4705,#4706);
#3814=AXIS2_PLACEMENT_3D('',#5756,#4710,#4711);
#3815=AXIS2_PLACEMENT_3D('',#5759,#4713,#4714);
#3816=AXIS2_PLACEMENT_3D('',#5760,#4715,#4716);
#3817=AXIS2_PLACEMENT_3D('',#5764,#4719,#4720);
#3818=AXIS2_PLACEMENT_3D('',#5772,#4724,#4725);
#3819=AXIS2_PLACEMENT_3D('',#5776,#4728,#4729);
#3820=AXIS2_PLACEMENT_3D('',#5780,#4732,#4733);
#3821=AXIS2_PLACEMENT_3D('',#5782,#4734,#4735);
#3822=AXIS2_PLACEMENT_3D('',#5784,#4737,#4738);
#3823=AXIS2_PLACEMENT_3D('',#5788,#4740,#4741);
#3824=AXIS2_PLACEMENT_3D('',#5792,#4743,#4744);
#3825=AXIS2_PLACEMENT_3D('',#5795,#4746,#4747);
#3826=AXIS2_PLACEMENT_3D('',#5799,#4749,#4750);
#3827=AXIS2_PLACEMENT_3D('',#5802,#4752,#4753);
#3828=AXIS2_PLACEMENT_3D('',#5803,#4754,#4755);
#3829=AXIS2_PLACEMENT_3D('',#5805,#4757,#4758);
#3830=AXIS2_PLACEMENT_3D('',#5807,#4760,#4761);
#3831=AXIS2_PLACEMENT_3D('',#5809,#4763,#4764);
#3832=AXIS2_PLACEMENT_3D('',#5812,#4767,#4768);
#3833=AXIS2_PLACEMENT_3D('',#5814,#4770,#4771);
#3834=AXIS2_PLACEMENT_3D('',#5816,#4773,#4774);
#3835=AXIS2_PLACEMENT_3D('',#5817,#4775,#4776);
#3836=AXIS2_PLACEMENT_3D('',#5819,#4778,#4779);
#3837=AXIS2_PLACEMENT_3D('',#5821,#4781,#4782);
#3838=AXIS2_PLACEMENT_3D('',#5823,#4784,#4785);
#3839=AXIS2_PLACEMENT_3D('',#5825,#4787,#4788);
#3840=AXIS2_PLACEMENT_3D('',#5829,#4791,#4792);
#3841=AXIS2_PLACEMENT_3D('',#5830,#4793,#4794);
#3842=AXIS2_PLACEMENT_3D('',#5831,#4795,#4796);
#3843=AXIS2_PLACEMENT_3D('',#5832,#4797,#4798);
#3844=AXIS2_PLACEMENT_3D('',#5834,#4799,#4800);
#3845=AXIS2_PLACEMENT_3D('',#5835,#4801,#4802);
#3846=AXIS2_PLACEMENT_3D('',#5837,#4803,#4804);
#3847=AXIS2_PLACEMENT_3D('',#5839,#4806,#4807);
#3848=AXIS2_PLACEMENT_3D('',#5840,#4808,#4809);
#3849=AXIS2_PLACEMENT_3D('',#5841,#4810,#4811);
#3850=AXIS2_PLACEMENT_3D('',#5843,#4812,#4813);
#3851=AXIS2_PLACEMENT_3D('',#5846,#4815,#4816);
#3852=AXIS2_PLACEMENT_3D('',#5847,#4817,#4818);
#3853=AXIS2_PLACEMENT_3D('',#5848,#4819,#4820);
#3854=AXIS2_PLACEMENT_3D('',#5849,#4821,#4822);
#3855=AXIS2_PLACEMENT_3D('',#5850,#4823,#4824);
#3856=AXIS2_PLACEMENT_3D('',#5852,#4825,#4826);
#3857=AXIS2_PLACEMENT_3D('',#5855,#4828,#4829);
#3858=AXIS2_PLACEMENT_3D('',#5856,#4830,#4831);
#3859=AXIS2_PLACEMENT_3D('',#5857,#4832,#4833);
#3860=AXIS2_PLACEMENT_3D('',#5858,#4834,#4835);
#3861=AXIS2_PLACEMENT_3D('',#5859,#4836,#4837);
#3862=AXIS2_PLACEMENT_3D('',#5861,#4838,#4839);
#3863=AXIS2_PLACEMENT_3D('',#5864,#4841,#4842);
#3864=AXIS2_PLACEMENT_3D('',#5865,#4843,#4844);
#3865=AXIS2_PLACEMENT_3D('',#5866,#4845,#4846);
#3866=AXIS2_PLACEMENT_3D('',#5867,#4847,#4848);
#3867=AXIS2_PLACEMENT_3D('',#5868,#4849,#4850);
#3868=AXIS2_PLACEMENT_3D('',#5870,#4851,#4852);
#3869=AXIS2_PLACEMENT_3D('',#5871,#4853,#4854);
#3870=AXIS2_PLACEMENT_3D('',#5873,#4855,#4856);
#3871=AXIS2_PLACEMENT_3D('',#5875,#4858,#4859);
#3872=AXIS2_PLACEMENT_3D('',#5876,#4860,#4861);
#3873=AXIS2_PLACEMENT_3D('',#5877,#4862,#4863);
#3874=AXIS2_PLACEMENT_3D('',#5879,#4864,#4865);
#3875=AXIS2_PLACEMENT_3D('',#5882,#4867,#4868);
#3876=AXIS2_PLACEMENT_3D('',#5883,#4869,#4870);
#3877=AXIS2_PLACEMENT_3D('',#5884,#4871,#4872);
#3878=AXIS2_PLACEMENT_3D('',#5885,#4873,#4874);
#3879=AXIS2_PLACEMENT_3D('',#5886,#4875,#4876);
#3880=AXIS2_PLACEMENT_3D('',#5887,#4877,#4878);
#3881=AXIS2_PLACEMENT_3D('',#5888,#4879,#4880);
#3882=AXIS2_PLACEMENT_3D('',#5889,#4881,#4882);
#3883=AXIS2_PLACEMENT_3D('',#5890,#4883,#4884);
#3884=AXIS2_PLACEMENT_3D('',#5891,#4885,#4886);
#3885=AXIS2_PLACEMENT_3D('',#5892,#4887,#4888);
#3886=DIRECTION('axis',(0.,0.,1.));
#3887=DIRECTION('refdir',(1.,0.,0.));
#3888=DIRECTION('axis',(0.,0.,1.));
#3889=DIRECTION('refdir',(1.,0.,0.));
#3890=DIRECTION('center_axis',(0.,-0.0208291764396898,0.999783049170591));
#3891=DIRECTION('ref_axis',(1.,0.,0.));
#3892=DIRECTION('',(-1.,0.,0.));
#3893=DIRECTION('center_axis',(0.,0.0208291764396898,-0.999783049170591));
#3894=DIRECTION('ref_axis',(1.,0.,0.));
#3895=DIRECTION('center_axis',(0.,0.0208291764396898,-0.999783049170591));
#3896=DIRECTION('ref_axis',(1.,0.,0.));
#3897=DIRECTION('center_axis',(0.,0.,-1.));
#3898=DIRECTION('ref_axis',(0.,-1.,0.));
#3899=DIRECTION('',(0.,0.0208291764396898,-0.999783049170591));
#3900=DIRECTION('center_axis',(0.,0.0208291764396907,0.999783049170591));
#3901=DIRECTION('ref_axis',(0.,-0.999783049170591,0.0208291764396907));
#3902=DIRECTION('center_axis',(0.,0.0208291764396907,0.999783049170591));
#3903=DIRECTION('ref_axis',(0.,-0.999783049170591,0.0208291764396907));
#3904=DIRECTION('center_axis',(0.,0.0208291764396898,-0.999783049170591));
#3905=DIRECTION('ref_axis',(1.,0.,0.));
#3906=DIRECTION('center_axis',(0.,0.0208291764396907,-0.999783049170591));
#3907=DIRECTION('ref_axis',(1.,0.,0.));
#3908=DIRECTION('',(0.,0.0208291764396898,-0.999783049170591));
#3909=DIRECTION('center_axis',(0.,0.,1.));
#3910=DIRECTION('ref_axis',(0.,-1.,0.));
#3911=DIRECTION('center_axis',(2.44876222201709E-16,-0.0208291764396898,
-0.999783049170591));
#3912=DIRECTION('ref_axis',(1.,-7.39048179408127E-33,2.44929359829471E-16));
#3913=DIRECTION('center_axis',(0.,0.,-1.));
#3914=DIRECTION('ref_axis',(0.,-1.,0.));
#3915=DIRECTION('center_axis',(4.67925299296849E-22,-0.707104673835204,
-0.707108888531611));
#3916=DIRECTION('ref_axis',(-1.73190695094883E-16,-0.707108888531611,0.707104673835204));
#3917=DIRECTION('center_axis',(0.,0.,-1.));
#3918=DIRECTION('ref_axis',(0.,-1.,0.));
#3919=DIRECTION('',(2.44876222201709E-16,-0.0208291764396898,-0.999783049170591));
#3920=DIRECTION('center_axis',(0.,0.,1.));
#3921=DIRECTION('ref_axis',(0.,-1.,0.));
#3922=DIRECTION('center_axis',(0.,0.,-1.));
#3923=DIRECTION('ref_axis',(1.,0.,0.));
#3924=DIRECTION('',(-1.,-6.61748276614988E-22,0.));
#3925=DIRECTION('',(0.,-1.,0.));
#3926=DIRECTION('',(-1.,0.,0.));
#3927=DIRECTION('',(0.,-1.,0.));
#3928=DIRECTION('',(-1.,-6.61748276614988E-22,0.));
#3929=DIRECTION('center_axis',(0.,1.,0.));
#3930=DIRECTION('ref_axis',(1.,0.,0.));
#3931=DIRECTION('center_axis',(0.,1.,0.));
#3932=DIRECTION('ref_axis',(1.,0.,0.));
#3933=DIRECTION('',(0.,1.,0.));
#3934=DIRECTION('center_axis',(0.,1.,0.));
#3935=DIRECTION('ref_axis',(1.,0.,0.));
#3936=DIRECTION('center_axis',(0.,-1.,0.));
#3937=DIRECTION('ref_axis',(1.,0.,0.));
#3938=DIRECTION('center_axis',(0.,1.,0.));
#3939=DIRECTION('ref_axis',(1.,0.,0.));
#3940=DIRECTION('center_axis',(0.,1.,0.));
#3941=DIRECTION('ref_axis',(1.,0.,0.));
#3942=DIRECTION('',(0.,1.,0.));
#3943=DIRECTION('center_axis',(0.,1.,0.));
#3944=DIRECTION('ref_axis',(1.,0.,0.));
#3945=DIRECTION('center_axis',(0.,-1.,0.));
#3946=DIRECTION('ref_axis',(1.,0.,0.));
#3947=DIRECTION('center_axis',(-1.,0.,0.));
#3948=DIRECTION('ref_axis',(0.,0.,-1.));
#3949=DIRECTION('',(0.,0.,1.));
#3950=DIRECTION('',(-1.7319121124633E-16,-0.707108888531611,0.707104673835204));
#3951=DIRECTION('',(-1.22464679914735E-16,-1.,0.));
#3952=DIRECTION('',(1.11022302462516E-16,0.,-1.));
#3953=DIRECTION('',(0.,1.,0.));
#3954=DIRECTION('center_axis',(-1.,0.,0.));
#3955=DIRECTION('ref_axis',(0.,0.,-1.));
#3956=DIRECTION('',(0.,0.,1.));
#3957=DIRECTION('',(0.,-1.,0.));
#3958=DIRECTION('',(1.11022302462516E-16,0.,-1.));
#3959=DIRECTION('',(1.22464679914735E-16,1.,0.));
#3960=DIRECTION('',(5.16151446404829E-22,0.707108888531611,0.707104673835204));
#3961=DIRECTION('',(0.,-1.,0.));
#3962=DIRECTION('center_axis',(0.,0.,-1.));
#3963=DIRECTION('ref_axis',(1.,0.,0.));
#3964=DIRECTION('',(1.,0.,-2.64892773006431E-15));
#3965=DIRECTION('',(0.,-1.,0.));
#3966=DIRECTION('',(0.,-1.,0.));
#3967=DIRECTION('',(1.,0.,0.));
#3968=DIRECTION('center_axis',(0.,1.,0.));
#3969=DIRECTION('ref_axis',(1.,0.,0.));
#3970=DIRECTION('center_axis',(0.,-1.,0.));
#3971=DIRECTION('ref_axis',(1.,0.,0.));
#3972=DIRECTION('center_axis',(0.,-1.,0.));
#3973=DIRECTION('ref_axis',(1.,0.,0.));
#3974=DIRECTION('',(0.,-1.,0.));
#3975=DIRECTION('center_axis',(0.,1.,0.));
#3976=DIRECTION('ref_axis',(1.,0.,0.));
#3977=DIRECTION('center_axis',(2.63841010085458E-15,0.,1.));
#3978=DIRECTION('ref_axis',(-1.,0.,2.63841010085458E-15));
#3979=DIRECTION('',(1.,0.,-2.63841010085458E-15));
#3980=DIRECTION('',(0.,-1.,0.));
#3981=DIRECTION('',(1.,0.,7.37272213361077E-17));
#3982=DIRECTION('',(0.,-1.,0.));
#3983=DIRECTION('',(-1.,0.,-7.37272213361077E-17));
#3984=DIRECTION('center_axis',(1.,0.,0.));
#3985=DIRECTION('ref_axis',(0.,0.,1.));
#3986=DIRECTION('',(0.,0.,-1.));
#3987=DIRECTION('',(0.,-1.,0.));
#3988=DIRECTION('',(0.,0.,1.));
#3989=DIRECTION('',(0.,-1.,0.));
#3990=DIRECTION('center_axis',(0.,-1.,0.));
#3991=DIRECTION('ref_axis',(-1.77635683940025E-15,0.,-1.));
#3992=DIRECTION('center_axis',(0.,-1.,0.));
#3993=DIRECTION('ref_axis',(-1.77635683940025E-15,0.,-1.));
#3994=DIRECTION('center_axis',(0.,1.,0.));
#3995=DIRECTION('ref_axis',(-1.77635683940025E-15,0.,-1.));
#3996=DIRECTION('center_axis',(0.,-1.,0.));
#3997=DIRECTION('ref_axis',(-1.99840144432528E-15,0.,-1.));
#3998=DIRECTION('center_axis',(0.,1.,0.));
#3999=DIRECTION('ref_axis',(-1.99840144432528E-15,0.,-1.));
#4000=DIRECTION('center_axis',(0.,-1.,0.));
#4001=DIRECTION('ref_axis',(-1.99840144432528E-15,0.,-1.));
#4002=DIRECTION('',(0.,-1.,0.));
#4003=DIRECTION('center_axis',(-1.,0.,0.));
#4004=DIRECTION('ref_axis',(0.,0.,-1.));
#4005=DIRECTION('',(0.,0.,-1.));
#4006=DIRECTION('',(0.,0.,-1.));
#4007=DIRECTION('',(0.,-1.,0.));
#4008=DIRECTION('center_axis',(-1.11022302462516E-16,1.35963107344689E-32,
1.));
#4009=DIRECTION('ref_axis',(1.22464679914735E-16,1.,1.64214663788065E-47));
#4010=DIRECTION('',(-1.,0.,-1.11022302462516E-16));
#4011=DIRECTION('',(-1.22464679914735E-16,-1.,0.));
#4012=DIRECTION('',(-1.,1.22464679914735E-16,-1.11022302462516E-16));
#4013=DIRECTION('center_axis',(-1.65100204443931E-16,-0.707104673835204,
0.707108888531611));
#4014=DIRECTION('ref_axis',(5.16151446398137E-22,0.707108888531611,0.707104673835204));
#4015=DIRECTION('',(-5.16151446404829E-22,-0.707108888531611,-0.707104673835204));
#4016=DIRECTION('',(1.,-2.33487644125528E-16,0.));
#4017=DIRECTION('center_axis',(4.67925299296849E-22,-0.707104673835204,
-0.707108888531611));
#4018=DIRECTION('ref_axis',(-1.7319121124633E-16,-0.707108888531611,0.707104673835204));
#4019=DIRECTION('',(1.7319121124633E-16,0.707108888531611,-0.707104673835204));
#4020=DIRECTION('',(-1.,1.11022302462516E-16,-1.11022302462516E-16));
#4021=DIRECTION('center_axis',(1.11022302462516E-16,-1.35963107344689E-32,
-1.));
#4022=DIRECTION('ref_axis',(-1.22464679914735E-16,-1.,-1.64214663788065E-47));
#4023=DIRECTION('',(1.22464679914735E-16,1.,0.));
#4024=DIRECTION('',(1.,0.,1.11022302462516E-16));
#4025=DIRECTION('center_axis',(0.,1.,0.));
#4026=DIRECTION('ref_axis',(1.,0.,0.));
#4027=DIRECTION('',(1.,0.,0.));
#4028=DIRECTION('',(0.,0.,-1.));
#4029=DIRECTION('',(1.,0.,-2.64892773006431E-15));
#4030=DIRECTION('center_axis',(0.,-1.,0.));
#4031=DIRECTION('ref_axis',(0.707106824182887,0.,0.707106738190206));
#4032=DIRECTION('',(-1.,0.,-7.37272213361077E-17));
#4033=DIRECTION('',(0.,0.,-1.));
#4034=DIRECTION('center_axis',(0.,-1.,0.));
#4035=DIRECTION('ref_axis',(-0.192330993613605,0.,0.981330112090526));
#4036=DIRECTION('center_axis',(0.,-1.,0.));
#4037=DIRECTION('ref_axis',(-0.192330993613605,0.,0.981330112090526));
#4038=DIRECTION('',(0.,-1.,0.));
#4039=DIRECTION('center_axis',(0.,1.,0.));
#4040=DIRECTION('ref_axis',(-0.192330993613605,0.,0.981330112090526));
#4041=DIRECTION('center_axis',(1.,0.,0.));
#4042=DIRECTION('ref_axis',(0.,0.,1.));
#4043=DIRECTION('',(0.,-1.,0.));
#4044=DIRECTION('',(0.,0.,1.));
#4045=DIRECTION('center_axis',(0.,0.,1.));
#4046=DIRECTION('ref_axis',(-1.,0.,0.));
#4047=DIRECTION('',(0.,-1.,0.));
#4048=DIRECTION('center_axis',(1.,0.,0.));
#4049=DIRECTION('ref_axis',(0.,0.,1.));
#4050=DIRECTION('',(-1.11022302462516E-16,0.,1.));
#4051=DIRECTION('',(0.,1.,0.));
#4052=DIRECTION('center_axis',(2.63841010085458E-15,0.,1.));
#4053=DIRECTION('ref_axis',(-1.,0.,2.63841010085458E-15));
#4054=DIRECTION('',(0.,-1.,0.));
#4055=DIRECTION('',(1.,0.,7.37272213361077E-17));
#4056=DIRECTION('',(0.,-1.,0.));
#4057=DIRECTION('',(1.,0.,-2.63841010085458E-15));
#4058=DIRECTION('center_axis',(0.,-1.,0.));
#4059=DIRECTION('ref_axis',(0.999999975140088,0.,0.000222979425697669));
#4060=DIRECTION('center_axis',(0.,-1.,0.));
#4061=DIRECTION('ref_axis',(0.999999975140088,0.,0.000222979425697669));
#4062=DIRECTION('center_axis',(0.,1.,0.));
#4063=DIRECTION('ref_axis',(0.999999975140088,0.,0.000222979425697669));
#4064=DIRECTION('',(0.,-1.,0.));
#4065=DIRECTION('center_axis',(-0.999999975140088,0.,-0.000222979425718608));
#4066=DIRECTION('ref_axis',(0.000222979425718608,0.,-0.999999975140088));
#4067=DIRECTION('',(-0.000222979425718608,0.,0.999999975140088));
#4068=DIRECTION('',(0.000222979425718608,0.,-0.999999975140088));
#4069=DIRECTION('',(0.,-1.,0.));
#4070=DIRECTION('center_axis',(0.,-1.,0.));
#4071=DIRECTION('ref_axis',(-0.149925588670012,0.,0.988697283227758));
#4072=DIRECTION('center_axis',(0.,-1.,0.));
#4073=DIRECTION('ref_axis',(-0.149925588670012,0.,0.988697283227758));
#4074=DIRECTION('center_axis',(0.,1.,0.));
#4075=DIRECTION('ref_axis',(-0.149925588670012,0.,0.988697283227758));
#4076=DIRECTION('center_axis',(0.602735860859126,0.,0.797940776019379));
#4077=DIRECTION('ref_axis',(-0.797940776019379,0.,0.602735860859126));
#4078=DIRECTION('',(0.797940776019378,0.,-0.602735860859126));
#4079=DIRECTION('',(-0.797940776019378,0.,0.602735860859126));
#4080=DIRECTION('',(0.,-1.,0.));
#4081=DIRECTION('center_axis',(0.,-1.,0.));
#4082=DIRECTION('ref_axis',(0.619814087082361,0.,0.784748684264115));
#4083=DIRECTION('center_axis',(0.,1.,0.));
#4084=DIRECTION('ref_axis',(0.619814087082361,0.,0.784748684264115));
#4085=DIRECTION('center_axis',(0.,-1.,0.));
#4086=DIRECTION('ref_axis',(0.619814087082361,0.,0.784748684264115));
#4087=DIRECTION('',(0.,-1.,0.));
#4088=DIRECTION('center_axis',(1.,0.,0.));
#4089=DIRECTION('ref_axis',(0.,0.,1.));
#4090=DIRECTION('',(0.,0.,1.));
#4091=DIRECTION('',(0.,0.,1.));
#4092=DIRECTION('',(0.,-1.,0.));
#4093=DIRECTION('center_axis',(0.,-1.,0.));
#4094=DIRECTION('ref_axis',(0.382683511888619,0.,-0.923879499571558));
#4095=DIRECTION('center_axis',(0.,1.,0.));
#4096=DIRECTION('ref_axis',(0.70710688994201,0.,0.707106672431068));
#4097=DIRECTION('center_axis',(0.,1.,0.));
#4098=DIRECTION('ref_axis',(0.70710688994201,0.,0.707106672431068));
#4099=DIRECTION('',(0.,1.,0.));
#4100=DIRECTION('center_axis',(0.,0.,-1.));
#4101=DIRECTION('ref_axis',(1.,0.,0.));
#4102=DIRECTION('',(1.,0.,0.));
#4103=DIRECTION('',(0.,-1.,0.));
#4104=DIRECTION('',(0.,-1.,0.));
#4105=DIRECTION('center_axis',(0.,-1.,0.));
#4106=DIRECTION('ref_axis',(0.707106824182887,0.,0.707106738190205));
#4107=DIRECTION('center_axis',(0.,1.,0.));
#4108=DIRECTION('ref_axis',(0.707106824182887,0.,0.707106738190205));
#4109=DIRECTION('',(0.,-1.,0.));
#4110=DIRECTION('center_axis',(0.,-1.,0.));
#4111=DIRECTION('ref_axis',(0.707106824182887,0.,0.707106738190205));
#4112=DIRECTION('center_axis',(0.,-1.,0.));
#4113=DIRECTION('ref_axis',(-0.70710688994201,0.,-0.707106672431068));
#4114=DIRECTION('center_axis',(0.,1.,0.));
#4115=DIRECTION('ref_axis',(-0.70710688994201,0.,-0.707106672431068));
#4116=DIRECTION('',(0.,-1.,0.));
#4117=DIRECTION('center_axis',(0.,-1.,0.));
#4118=DIRECTION('ref_axis',(-0.70710688994201,0.,-0.707106672431068));
#4119=DIRECTION('center_axis',(0.,-1.,0.));
#4120=DIRECTION('ref_axis',(-0.70710688994201,0.,-0.707106672431068));
#4121=DIRECTION('',(0.,-1.,0.));
#4122=DIRECTION('center_axis',(0.707106955701123,0.,0.707106606671929));
#4123=DIRECTION('ref_axis',(-0.707106606671929,0.,0.707106955701123));
#4124=DIRECTION('',(0.707106606671929,0.,-0.707106955701123));
#4125=DIRECTION('',(0.,-1.,0.));
#4126=DIRECTION('',(-0.707106606671929,0.,0.707106955701123));
#4127=DIRECTION('center_axis',(0.,-1.,0.));
#4128=DIRECTION('ref_axis',(-0.382683511888619,0.,0.923879499571558));
#4129=DIRECTION('center_axis',(0.,1.,0.));
#4130=DIRECTION('ref_axis',(-0.70710688994201,0.,-0.707106672431068));
#4131=DIRECTION('',(0.,-1.,0.));
#4132=DIRECTION('center_axis',(0.,1.,0.));
#4133=DIRECTION('ref_axis',(-0.70710688994201,0.,-0.707106672431068));
#4134=DIRECTION('center_axis',(-1.,0.,0.));
#4135=DIRECTION('ref_axis',(0.,0.,-1.));
#4136=DIRECTION('',(0.,0.,-1.));
#4137=DIRECTION('',(0.,-1.,0.));
#4138=DIRECTION('',(0.,0.,-1.));
#4139=DIRECTION('center_axis',(0.,-1.,0.));
#4140=DIRECTION('ref_axis',(-0.619814087082361,0.,-0.784748684264115));
#4141=DIRECTION('center_axis',(0.,1.,0.));
#4142=DIRECTION('ref_axis',(-0.619814087082361,0.,-0.784748684264115));
#4143=DIRECTION('',(0.,-1.,0.));
#4144=DIRECTION('center_axis',(0.,-1.,0.));
#4145=DIRECTION('ref_axis',(-0.619814087082361,0.,-0.784748684264115));
#4146=DIRECTION('center_axis',(0.999999975140088,0.,0.000222979425718608));
#4147=DIRECTION('ref_axis',(-0.000222979425718608,0.,0.999999975140088));
#4148=DIRECTION('',(0.000222979425718608,0.,-0.999999975140088));
#4149=DIRECTION('',(0.,-1.,0.));
#4150=DIRECTION('',(-0.000222979425718608,0.,0.999999975140088));
#4151=DIRECTION('',(0.,-1.,0.));
#4152=DIRECTION('center_axis',(0.,-1.,0.));
#4153=DIRECTION('ref_axis',(-0.999999975140088,0.,-0.000222979425691007));
#4154=DIRECTION('center_axis',(0.,-1.,0.));
#4155=DIRECTION('ref_axis',(-0.999999975140088,0.,-0.000222979425691007));
#4156=DIRECTION('',(0.,-1.,0.));
#4157=DIRECTION('center_axis',(0.,1.,0.));
#4158=DIRECTION('ref_axis',(-0.999999975140088,0.,-0.000222979425691007));
#4159=DIRECTION('center_axis',(0.,-1.,0.));
#4160=DIRECTION('ref_axis',(-0.707106824182888,0.,-0.707106738190205));
#4161=DIRECTION('',(0.,-1.,0.));
#4162=DIRECTION('center_axis',(0.,-1.,0.));
#4163=DIRECTION('ref_axis',(-0.707106824182888,0.,-0.707106738190205));
#4164=DIRECTION('',(0.,-1.,0.));
#4165=DIRECTION('center_axis',(-1.,0.,0.));
#4166=DIRECTION('ref_axis',(0.,0.,1.));
#4167=DIRECTION('',(0.,0.,1.));
#4168=DIRECTION('',(0.,-1.,0.));
#4169=DIRECTION('',(0.,0.,1.));
#4170=DIRECTION('',(0.,1.,0.));
#4171=DIRECTION('center_axis',(-1.,0.,0.));
#4172=DIRECTION('ref_axis',(0.,0.,1.));
#4173=DIRECTION('',(0.,0.,1.));
#4174=DIRECTION('',(0.,1.,0.));
#4175=DIRECTION('',(0.,0.,1.));
#4176=DIRECTION('',(0.,1.,0.));
#4177=DIRECTION('center_axis',(-1.,0.,0.));
#4178=DIRECTION('ref_axis',(0.,0.,1.));
#4179=DIRECTION('',(0.,0.,1.));
#4180=DIRECTION('',(0.,0.999783049170591,0.0208291764396907));
#4181=DIRECTION('',(0.,0.,1.));
#4182=DIRECTION('',(0.,-1.,0.));
#4183=DIRECTION('',(0.,-0.707108888531611,-0.707104673835204));
#4184=DIRECTION('',(0.,-0.707108888531611,0.707104673835204));
#4185=DIRECTION('center_axis',(-1.,0.,0.));
#4186=DIRECTION('ref_axis',(0.,0.,1.));
#4187=DIRECTION('',(0.,0.,1.));
#4188=DIRECTION('',(0.,0.707108888531611,0.707104673835204));
#4189=DIRECTION('',(0.,0.707108888531611,-0.707104673835204));
#4190=DIRECTION('',(0.,1.,0.));
#4191=DIRECTION('',(0.,0.,1.));
#4192=DIRECTION('',(0.,-0.999783049170591,0.0208291764396907));
#4193=DIRECTION('center_axis',(-0.707106889942011,0.,-0.707106672431068));
#4194=DIRECTION('ref_axis',(0.707106672431068,0.,-0.707106889942011));
#4195=DIRECTION('',(0.707106672431068,0.,-0.70710688994201));
#4196=DIRECTION('',(0.707106672431068,0.,-0.70710688994201));
#4197=DIRECTION('center_axis',(0.,-1.,0.));
#4198=DIRECTION('ref_axis',(0.192330993613606,0.,-0.981330112090525));
#4199=DIRECTION('center_axis',(0.,1.,0.));
#4200=DIRECTION('ref_axis',(0.192330993613606,0.,-0.981330112090525));
#4201=DIRECTION('',(0.,-1.,0.));
#4202=DIRECTION('center_axis',(0.,-1.,0.));
#4203=DIRECTION('ref_axis',(0.192330993613606,0.,-0.981330112090525));
#4204=DIRECTION('center_axis',(1.,0.,0.));
#4205=DIRECTION('ref_axis',(0.,0.,1.));
#4206=DIRECTION('',(0.,0.,-1.));
#4207=DIRECTION('',(0.,-1.,0.));
#4208=DIRECTION('',(0.,0.,1.));
#4209=DIRECTION('center_axis',(0.,-1.,0.));
#4210=DIRECTION('ref_axis',(0.,0.,1.));
#4211=DIRECTION('center_axis',(0.,1.,0.));
#4212=DIRECTION('ref_axis',(0.,0.,1.));
#4213=DIRECTION('',(0.,-1.,0.));
#4214=DIRECTION('center_axis',(0.,-1.,0.));
#4215=DIRECTION('ref_axis',(0.,0.,1.));
#4216=DIRECTION('',(0.,-1.,0.));
#4217=DIRECTION('center_axis',(0.,0.,1.));
#4218=DIRECTION('ref_axis',(-1.,0.,0.));
#4219=DIRECTION('',(1.,0.,0.));
#4220=DIRECTION('',(1.,0.,0.));
#4221=DIRECTION('',(0.,-1.,0.));
#4222=DIRECTION('',(-1.,0.,2.56034438634048E-15));
#4223=DIRECTION('',(-1.,0.,0.));
#4224=DIRECTION('',(-1.,0.,2.56034438634048E-15));
#4225=DIRECTION('',(1.,0.,0.));
#4226=DIRECTION('center_axis',(0.,-1.,0.));
#4227=DIRECTION('ref_axis',(0.,0.,1.));
#4228=DIRECTION('center_axis',(0.,-1.,0.));
#4229=DIRECTION('ref_axis',(0.,0.,1.));
#4230=DIRECTION('',(0.,-1.,0.));
#4231=DIRECTION('center_axis',(0.,1.,0.));
#4232=DIRECTION('ref_axis',(0.,0.,1.));
#4233=DIRECTION('',(0.,-1.,0.));
#4234=DIRECTION('center_axis',(-1.,0.,0.));
#4235=DIRECTION('ref_axis',(0.,0.,-1.));
#4236=DIRECTION('',(0.,0.,1.));
#4237=DIRECTION('',(0.,-1.,0.));
#4238=DIRECTION('',(0.,0.,-1.));
#4239=DIRECTION('center_axis',(0.,1.,0.));
#4240=DIRECTION('ref_axis',(1.,0.,0.));
#4241=DIRECTION('',(-1.,0.,2.63527591935953E-15));
#4242=DIRECTION('center_axis',(0.,1.,0.));
#4243=DIRECTION('ref_axis',(0.149925588670012,0.,-0.988697283227758));
#4244=DIRECTION('',(-1.,0.,2.63527591935953E-15));
#4245=DIRECTION('center_axis',(0.,-1.,0.));
#4246=DIRECTION('ref_axis',(1.,0.,0.));
#4247=DIRECTION('center_axis',(0.,-1.,0.));
#4248=DIRECTION('ref_axis',(1.,0.,0.));
#4249=DIRECTION('',(0.,-1.,0.));
#4250=DIRECTION('center_axis',(0.,1.,0.));
#4251=DIRECTION('ref_axis',(1.,0.,0.));
#4252=DIRECTION('center_axis',(0.,1.,0.));
#4253=DIRECTION('ref_axis',(1.,0.,0.));
#4254=DIRECTION('center_axis',(1.,0.,0.));
#4255=DIRECTION('ref_axis',(0.,0.,-1.));
#4256=DIRECTION('',(0.,0.,-1.));
#4257=DIRECTION('',(0.,1.,0.));
#4258=DIRECTION('',(0.,0.,-1.));
#4259=DIRECTION('',(0.,1.,0.));
#4260=DIRECTION('center_axis',(0.,1.,0.));
#4261=DIRECTION('ref_axis',(0.,0.,1.));
#4262=DIRECTION('',(-1.,0.,0.));
#4263=DIRECTION('',(0.,0.,-1.));
#4264=DIRECTION('',(0.,0.,-1.));
#4265=DIRECTION('',(-1.,0.,0.));
#4266=DIRECTION('center_axis',(1.,0.,0.));
#4267=DIRECTION('ref_axis',(0.,0.,-1.));
#4268=DIRECTION('',(0.,0.,-1.));
#4269=DIRECTION('',(0.,1.,0.));
#4270=DIRECTION('center_axis',(0.,0.,-1.));
#4271=DIRECTION('ref_axis',(-1.,0.,0.));
#4272=DIRECTION('',(-1.,0.,0.));
#4273=DIRECTION('center_axis',(0.,-1.,0.));
#4274=DIRECTION('ref_axis',(0.,0.,1.));
#4275=DIRECTION('',(1.,0.,0.));
#4276=DIRECTION('',(0.,0.,-1.));
#4277=DIRECTION('',(-1.,0.,0.));
#4278=DIRECTION('center_axis',(0.,-0.0208291764396907,0.999783049170591));
#4279=DIRECTION('ref_axis',(0.,0.999783049170591,0.0208291764396907));
#4280=DIRECTION('',(0.,-0.999783049170591,-0.0208291764396907));
#4281=DIRECTION('center_axis',(0.,0.,-1.));
#4282=DIRECTION('ref_axis',(0.,-1.,0.));
#4283=DIRECTION('',(0.,1.,0.));
#4284=DIRECTION('',(-1.,0.,0.));
#4285=DIRECTION('center_axis',(0.,0.707104673835204,-0.707108888531611));
#4286=DIRECTION('ref_axis',(0.,-0.707108888531611,-0.707104673835204));
#4287=DIRECTION('',(0.,0.707108888531611,0.707104673835204));
#4288=DIRECTION('',(-1.,0.,0.));
#4289=DIRECTION('center_axis',(0.,-0.707104673835204,-0.707108888531611));
#4290=DIRECTION('ref_axis',(0.,-0.707108888531611,0.707104673835204));
#4291=DIRECTION('',(0.,0.707108888531611,-0.707104673835204));
#4292=DIRECTION('center_axis',(1.,0.,0.));
#4293=DIRECTION('ref_axis',(0.,0.,-1.));
#4294=DIRECTION('center_axis',(1.,0.,0.));
#4295=DIRECTION('ref_axis',(0.,0.,-1.));
#4296=DIRECTION('',(0.,0.,-1.));
#4297=DIRECTION('',(0.,0.999783049170591,-0.0208291764396907));
#4298=DIRECTION('',(0.,0.,-1.));
#4299=DIRECTION('',(0.,-1.,0.));
#4300=DIRECTION('',(0.,-0.707108888531611,0.707104673835204));
#4301=DIRECTION('',(0.,-0.707108888531611,-0.707104673835204));
#4302=DIRECTION('center_axis',(0.,1.,0.));
#4303=DIRECTION('ref_axis',(1.,0.,0.));
#4304=DIRECTION('center_axis',(0.,-1.,0.));
#4305=DIRECTION('ref_axis',(0.149925588670012,0.,-0.988697283227758));
#4306=DIRECTION('',(-1.,0.,2.72352010410795E-15));
#4307=DIRECTION('center_axis',(0.,-1.,0.));
#4308=DIRECTION('ref_axis',(0.149925588670012,0.,-0.988697283227758));
#4309=DIRECTION('center_axis',(-2.72352010410795E-15,0.,-1.));
#4310=DIRECTION('ref_axis',(1.,0.,-2.72352010410795E-15));
#4311=DIRECTION('',(1.,0.,-2.63527591935953E-15));
#4312=DIRECTION('',(-1.,0.,2.72352010410795E-15));
#4313=DIRECTION('',(-1.,0.,2.72352010410795E-15));
#4314=DIRECTION('',(-1.,0.,2.72352010410795E-15));
#4315=DIRECTION('',(1.,0.,-2.63527591935953E-15));
#4316=DIRECTION('center_axis',(0.,-0.0208291764396907,-0.999783049170591));
#4317=DIRECTION('ref_axis',(0.,-0.999783049170591,0.0208291764396907));
#4318=DIRECTION('',(1.,0.,0.));
#4319=DIRECTION('center_axis',(0.,-1.,0.));
#4320=DIRECTION('ref_axis',(0.,0.,1.));
#4321=DIRECTION('',(-1.,0.,0.));
#4322=DIRECTION('center_axis',(0.,-0.707104673835204,0.707108888531611));
#4323=DIRECTION('ref_axis',(0.,0.707108888531611,0.707104673835204));
#4324=DIRECTION('',(-1.,0.,0.));
#4325=DIRECTION('center_axis',(0.,0.707104673835204,0.707108888531611));
#4326=DIRECTION('ref_axis',(0.,0.707108888531611,-0.707104673835204));
#4327=DIRECTION('',(-1.,0.,0.));
#4328=DIRECTION('center_axis',(0.,0.,1.));
#4329=DIRECTION('ref_axis',(0.,1.,0.));
#4330=DIRECTION('',(1.,0.,0.));
#4331=DIRECTION('center_axis',(0.,1.,0.));
#4332=DIRECTION('ref_axis',(0.,0.,1.));
#4333=DIRECTION('',(1.,0.,0.));
#4334=DIRECTION('center_axis',(0.,0.,1.));
#4335=DIRECTION('ref_axis',(1.,0.,0.));
#4336=DIRECTION('',(1.,0.,0.));
#4337=DIRECTION('center_axis',(0.,1.,0.));
#4338=DIRECTION('ref_axis',(1.,0.,0.));
#4339=DIRECTION('axis',(0.,0.,1.));
#4340=DIRECTION('refdir',(1.,0.,0.));
#4341=DIRECTION('center_axis',(-2.44876222201709E-16,0.0208291764396898,
0.999783049170591));
#4342=DIRECTION('ref_axis',(1.,-7.39048179408127E-33,2.44929359829471E-16));
#4343=DIRECTION('',(1.,2.87786876793731E-15,1.84972715848191E-16));
#4344=DIRECTION('center_axis',(-2.44876222201709E-16,0.0208291764396898,
0.999783049170591));
#4345=DIRECTION('ref_axis',(1.,-7.39048179408127E-33,2.44929359829471E-16));
#4346=DIRECTION('center_axis',(2.44876222201709E-16,-0.0208291764396898,
-0.999783049170591));
#4347=DIRECTION('ref_axis',(1.,-7.39048179408127E-33,2.44929359829471E-16));
#4348=DIRECTION('center_axis',(1.22464679914735E-16,0.,-1.));
#4349=DIRECTION('ref_axis',(0.,-1.,0.));
#4350=DIRECTION('center_axis',(1.7319121124633E-16,0.707104673835204,-0.707108888531611));
#4351=DIRECTION('ref_axis',(1.73190695094883E-16,-0.707108888531611,-0.707104673835204));
#4352=DIRECTION('center_axis',(1.22464679914735E-16,0.,-1.));
#4353=DIRECTION('ref_axis',(0.,-1.,0.));
#4354=DIRECTION('',(2.44876222201709E-16,-0.0208291764396898,-0.999783049170591));
#4355=DIRECTION('center_axis',(-1.24988949526429E-16,-0.0208291764396907,
0.999783049170591));
#4356=DIRECTION('ref_axis',(5.10167685114853E-18,-0.999783049170591,-0.0208291764396907));
#4357=DIRECTION('center_axis',(-1.24988949526429E-16,-0.0208291764396907,
0.999783049170591));
#4358=DIRECTION('ref_axis',(5.10167685114853E-18,-0.999783049170591,-0.0208291764396907));
#4359=DIRECTION('center_axis',(2.44876222201709E-16,-0.0208291764396898,
-0.999783049170591));
#4360=DIRECTION('ref_axis',(1.,-7.39048179408127E-33,2.44929359829471E-16));
#4361=DIRECTION('center_axis',(1.1988727267528E-16,-0.0208291764396907,
-0.999783049170591));
#4362=DIRECTION('ref_axis',(1.,-2.60341688269759E-18,1.19967526759308E-16));
#4363=DIRECTION('',(2.44876222201709E-16,-0.0208291764396898,-0.999783049170591));
#4364=DIRECTION('center_axis',(-1.22464679914735E-16,0.,1.));
#4365=DIRECTION('ref_axis',(0.,-1.,0.));
#4366=DIRECTION('center_axis',(-5.16151446417155E-22,0.707104673835204,
0.707108888531611));
#4367=DIRECTION('ref_axis',(-1.73190695094883E-16,-0.707108888531611,0.707104673835204));
#4368=DIRECTION('center_axis',(-1.22464679914735E-16,0.,1.));
#4369=DIRECTION('ref_axis',(0.,-1.,0.));
#4370=DIRECTION('center_axis',(1.22464679914735E-16,0.,-1.));
#4371=DIRECTION('ref_axis',(-1.22464679914735E-16,-1.,-1.49975978266185E-32));
#4372=DIRECTION('',(-1.,1.22464679914735E-16,-1.22464679914735E-16));
#4373=DIRECTION('',(1.22464679914735E-16,1.,1.49975978266186E-32));
#4374=DIRECTION('',(1.,-1.22464679914735E-16,1.22464679914735E-16));
#4375=DIRECTION('',(-1.22464679914735E-16,-1.,-1.49975978266186E-32));
#4376=DIRECTION('',(-1.,1.22464679914735E-16,-1.22464679914735E-16));
#4377=DIRECTION('center_axis',(-1.22464679914735E-16,0.,1.));
#4378=DIRECTION('ref_axis',(1.22464679914735E-16,1.,1.49975978266185E-32));
#4379=DIRECTION('',(-1.,1.22464679914735E-16,-1.22464679914735E-16));
#4380=DIRECTION('',(1.22464679914735E-16,1.,1.49975978266186E-32));
#4381=DIRECTION('',(-1.,1.22464679914735E-16,-1.22464679914735E-16));
#4382=DIRECTION('',(-1.22464679914735E-16,-1.,-1.49975978266186E-32));
#4383=DIRECTION('',(-1.,1.22464679914735E-16,-1.22464679914735E-16));
#4384=DIRECTION('center_axis',(0.,0.0208291764396898,-0.999783049170591));
#4385=DIRECTION('ref_axis',(1.,0.,0.));
#4386=DIRECTION('center_axis',(1.22464679914735E-16,0.,-1.));
#4387=DIRECTION('ref_axis',(0.,-1.,0.));
#4388=DIRECTION('',(0.,0.0208291764396898,-0.999783049170591));
#4389=DIRECTION('center_axis',(-1.22464679914735E-16,0.,1.));
#4390=DIRECTION('ref_axis',(0.,-1.,0.));
#4391=DIRECTION('center_axis',(0.,-1.,0.));
#4392=DIRECTION('ref_axis',(-1.,0.,0.));
#4393=DIRECTION('center_axis',(-1.22464679914735E-16,-1.,-1.49975978266186E-32));
#4394=DIRECTION('ref_axis',(1.,-1.22464679914735E-16,1.22464679914735E-16));
#4395=DIRECTION('',(0.,-1.,0.));
#4396=DIRECTION('center_axis',(1.83667601732677E-48,-1.,2.73691106313441E-48));
#4397=DIRECTION('ref_axis',(-1.,-1.83667601732677E-48,0.));
#4398=DIRECTION('center_axis',(-1.83667601732677E-48,1.,-2.73691106313441E-48));
#4399=DIRECTION('ref_axis',(-1.,-1.83667601732677E-48,0.));
#4400=DIRECTION('center_axis',(0.,-1.,0.));
#4401=DIRECTION('ref_axis',(-1.,0.,0.));
#4402=DIRECTION('center_axis',(-1.22464679914735E-16,-1.,-1.49975978266186E-32));
#4403=DIRECTION('ref_axis',(1.,-1.22464679914735E-16,1.22464679914735E-16));
#4404=DIRECTION('',(0.,-1.,0.));
#4405=DIRECTION('center_axis',(1.83667601732677E-48,-1.,2.24927940568994E-64));
#4406=DIRECTION('ref_axis',(-1.,-1.83667601732677E-48,0.));
#4407=DIRECTION('center_axis',(-1.83667601732677E-48,1.,-2.24927940568994E-64));
#4408=DIRECTION('ref_axis',(-1.,-1.83667601732677E-48,0.));
#4409=DIRECTION('center_axis',(1.,-1.22464679914735E-16,1.22464679914735E-16));
#4410=DIRECTION('ref_axis',(1.22464679914735E-16,0.,-1.));
#4411=DIRECTION('',(-1.22464679914735E-16,0.,1.));
#4412=DIRECTION('',(1.22464679914735E-16,1.,1.49975978266186E-32));
#4413=DIRECTION('',(1.22464679914735E-16,0.,-1.));
#4414=DIRECTION('',(1.22464679914735E-16,1.,1.49975978266186E-32));
#4415=DIRECTION('center_axis',(1.22464679914735E-16,1.,1.49975978266186E-32));
#4416=DIRECTION('ref_axis',(1.22464679914735E-16,1.0252425757274E-46,-1.));
#4417=DIRECTION('center_axis',(-1.22464679914735E-16,-1.,-1.49975978266186E-32));
#4418=DIRECTION('ref_axis',(1.22464679914735E-16,1.0252425757274E-46,-1.));
#4419=DIRECTION('',(1.22464679914735E-16,1.,1.49975978266186E-32));
#4420=DIRECTION('center_axis',(1.22464679914735E-16,1.,1.49975978266186E-32));
#4421=DIRECTION('ref_axis',(1.22464679914735E-16,1.0252425757274E-46,-1.));
#4422=DIRECTION('',(1.22464679914735E-16,1.,1.49975978266186E-32));
#4423=DIRECTION('center_axis',(1.22464679914735E-16,1.,1.49975978266186E-32));
#4424=DIRECTION('ref_axis',(1.22464679914735E-16,1.0252425757274E-46,-1.));
#4425=DIRECTION('center_axis',(1.22464679914735E-16,1.,1.49975978266186E-32));
#4426=DIRECTION('ref_axis',(1.22464679914735E-16,1.0252425757274E-46,-1.));
#4427=DIRECTION('',(1.22464679914735E-16,1.,1.49975978266186E-32));
#4428=DIRECTION('center_axis',(-1.22464679914735E-16,-1.,-1.49975978266186E-32));
#4429=DIRECTION('ref_axis',(1.22464679914735E-16,1.0252425757274E-46,-1.));
#4430=DIRECTION('',(1.22464679914735E-16,1.,1.49975978266186E-32));
#4431=DIRECTION('center_axis',(-1.,1.22464679914735E-16,-1.22464679914735E-16));
#4432=DIRECTION('ref_axis',(-1.22464679914735E-16,0.,1.));
#4433=DIRECTION('',(1.22464679914735E-16,0.,-1.));
#4434=DIRECTION('',(1.22464679914735E-16,1.,1.49975978266186E-32));
#4435=DIRECTION('',(-1.22464679914735E-16,0.,1.));
#4436=DIRECTION('center_axis',(1.22464679914735E-16,1.,1.49975978266186E-32));
#4437=DIRECTION('ref_axis',(1.,-1.22464679914735E-16,1.22464679914735E-16));
#4438=DIRECTION('center_axis',(1.22464679914735E-16,1.,1.49975978266186E-32));
#4439=DIRECTION('ref_axis',(1.,-1.22464679914735E-16,1.22464679914735E-16));
#4440=DIRECTION('',(1.22464679914735E-16,1.,1.49975978266186E-32));
#4441=DIRECTION('center_axis',(-1.22464679914735E-16,-1.,-1.49975978266186E-32));
#4442=DIRECTION('ref_axis',(1.,-1.22464679914735E-16,1.22464679914735E-16));
#4443=DIRECTION('center_axis',(-1.22464679914735E-16,-1.,-1.49975978266186E-32));
#4444=DIRECTION('ref_axis',(1.,-1.22464679914735E-16,1.22464679914735E-16));
#4445=DIRECTION('center_axis',(1.,-1.22464679914735E-16,1.22464679914735E-16));
#4446=DIRECTION('ref_axis',(-1.22464679914735E-16,0.,1.));
#4447=DIRECTION('',(-1.22464679914735E-16,0.,1.));
#4448=DIRECTION('',(-1.22464679914735E-16,-1.,-1.49975978266186E-32));
#4449=DIRECTION('',(-1.22464679914735E-16,0.,1.));
#4450=DIRECTION('',(-1.22464679914735E-16,-1.,-1.49975978266186E-32));
#4451=DIRECTION('center_axis',(1.,-1.22464679914735E-16,1.22464679914735E-16));
#4452=DIRECTION('ref_axis',(-1.22464679914735E-16,0.,1.));
#4453=DIRECTION('',(-1.22464679914735E-16,0.,1.));
#4454=DIRECTION('',(1.22464679914735E-16,1.,1.49975978266186E-32));
#4455=DIRECTION('',(-1.22464679914735E-16,0.,1.));
#4456=DIRECTION('',(-1.22464679914735E-16,-1.,-1.49975978266186E-32));
#4457=DIRECTION('center_axis',(1.,-1.22464679914735E-16,1.22464679914735E-16));
#4458=DIRECTION('ref_axis',(-1.22464679914735E-16,0.,1.));
#4459=DIRECTION('',(-1.22464679914735E-16,0.,1.));
#4460=DIRECTION('',(-1.7319121124633E-16,-0.707108888531611,0.707104673835204));
#4461=DIRECTION('',(-5.16151446417155E-22,-0.707108888531611,-0.707104673835204));
#4462=DIRECTION('',(-1.22464679914735E-16,0.,1.));
#4463=DIRECTION('',(1.1988727267528E-16,0.999783049170591,0.0208291764396907));
#4464=DIRECTION('center_axis',(1.,-1.22464679914735E-16,1.22464679914735E-16));
#4465=DIRECTION('ref_axis',(-1.22464679914735E-16,0.,1.));
#4466=DIRECTION('',(-1.22464679914735E-16,0.,1.));
#4467=DIRECTION('',(-1.24988949526429E-16,-0.999783049170591,0.0208291764396907));
#4468=DIRECTION('',(-1.22464679914735E-16,0.,1.));
#4469=DIRECTION('',(1.7319121124633E-16,0.707108888531611,-0.707104673835204));
#4470=DIRECTION('',(5.16151446417155E-22,0.707108888531611,0.707104673835204));
#4471=DIRECTION('center_axis',(1.22464679914735E-16,1.,1.49975978266186E-32));
#4472=DIRECTION('ref_axis',(-0.70710688994201,8.6595618942252E-17,0.707106672431068));
#4473=DIRECTION('center_axis',(-1.22464679914735E-16,-1.,-1.49975978266186E-32));
#4474=DIRECTION('ref_axis',(-0.70710688994201,8.6595618942252E-17,0.707106672431068));
#4475=DIRECTION('',(1.22464679914735E-16,1.,1.49975978266186E-32));
#4476=DIRECTION('center_axis',(1.22464679914735E-16,1.,1.49975978266186E-32));
#4477=DIRECTION('ref_axis',(-0.70710688994201,8.6595618942252E-17,0.707106672431068));
#4478=DIRECTION('center_axis',(1.22464679914735E-16,1.,1.49975978266186E-32));
#4479=DIRECTION('ref_axis',(-0.70710688994201,8.6595618942252E-17,0.707106672431068));
#4480=DIRECTION('',(1.22464679914735E-16,1.,1.49975978266186E-32));
#4481=DIRECTION('center_axis',(1.22464679914735E-16,1.,1.49975978266186E-32));
#4482=DIRECTION('ref_axis',(-0.382683511888619,4.68652137920864E-17,-0.923879499571558));
#4483=DIRECTION('center_axis',(-1.22464679914735E-16,-1.,-1.49975978266186E-32));
#4484=DIRECTION('ref_axis',(-0.70710688994201,8.6595618942252E-17,0.707106672431068));
#4485=DIRECTION('',(1.22464679914735E-16,1.,1.49975978266186E-32));
#4486=DIRECTION('center_axis',(-1.22464679914735E-16,-1.,-1.49975978266186E-32));
#4487=DIRECTION('ref_axis',(-0.70710688994201,8.6595618942252E-17,0.707106672431068));
#4488=DIRECTION('',(1.22464679914735E-16,1.,1.49975978266186E-32));
#4489=DIRECTION('center_axis',(-1.,1.22464679914735E-16,-1.22464679914735E-16));
#4490=DIRECTION('ref_axis',(-1.22464679914735E-16,0.,1.));
#4491=DIRECTION('',(-1.22464679914735E-16,0.,1.));
#4492=DIRECTION('',(1.22464679914735E-16,1.,1.49975978266186E-32));
#4493=DIRECTION('',(-1.22464679914735E-16,0.,1.));
#4494=DIRECTION('center_axis',(1.22464679914735E-16,1.,1.49975978266186E-32));
#4495=DIRECTION('ref_axis',(-0.619814087082361,7.5905333781185E-17,0.784748684264115));
#4496=DIRECTION('center_axis',(-1.22464679914735E-16,-1.,-1.49975978266186E-32));
#4497=DIRECTION('ref_axis',(-0.619814087082361,7.5905333781185E-17,0.784748684264115));
#4498=DIRECTION('',(1.22464679914735E-16,1.,1.49975978266186E-32));
#4499=DIRECTION('center_axis',(1.22464679914735E-16,1.,1.49975978266186E-32));
#4500=DIRECTION('ref_axis',(-0.619814087082361,7.5905333781185E-17,0.784748684264115));
#4501=DIRECTION('center_axis',(1.22464679914735E-16,1.,1.49975978266186E-32));
#4502=DIRECTION('ref_axis',(0.149925588670012,-1.83605892275013E-17,0.988697283227758));
#4503=DIRECTION('center_axis',(1.22464679914735E-16,1.,1.49975978266186E-32));
#4504=DIRECTION('ref_axis',(0.149925588670012,-1.83605892275013E-17,0.988697283227758));
#4505=DIRECTION('',(1.22464679914735E-16,1.,1.49975978266186E-32));
#4506=DIRECTION('center_axis',(-1.22464679914735E-16,-1.,-1.49975978266186E-32));
#4507=DIRECTION('ref_axis',(0.149925588670012,-1.83605892275013E-17,0.988697283227758));
#4508=DIRECTION('center_axis',(0.999999975140088,-1.22464676870274E-16,
-0.000222979425718486));
#4509=DIRECTION('ref_axis',(-0.000222979425718486,2.73071039982008E-20,
-0.999999975140088));
#4510=DIRECTION('',(0.000222979425718486,-2.73071039982008E-20,0.999999975140088));
#4511=DIRECTION('',(1.22464679914735E-16,1.,1.49975978266186E-32));
#4512=DIRECTION('',(-0.000222979425718486,2.73071039982008E-20,-0.999999975140088));
#4513=DIRECTION('center_axis',(1.22464679914735E-16,1.,1.49975978266186E-32));
#4514=DIRECTION('ref_axis',(-0.999999975140088,1.22464676870274E-16,0.000222979425690885));
#4515=DIRECTION('center_axis',(1.22464679914735E-16,1.,1.49975978266186E-32));
#4516=DIRECTION('ref_axis',(-0.999999975140088,1.22464676870274E-16,0.000222979425690885));
#4517=DIRECTION('',(1.22464679914735E-16,1.,1.49975978266186E-32));
#4518=DIRECTION('center_axis',(-1.22464679914735E-16,-1.,-1.49975978266186E-32));
#4519=DIRECTION('ref_axis',(-0.999999975140088,1.22464676870274E-16,0.000222979425690885));
#4520=DIRECTION('center_axis',(-2.84598478402269E-15,3.33535017790927E-31,
1.));
#4521=DIRECTION('ref_axis',(1.,-1.22464679914735E-16,2.84598478402269E-15));
#4522=DIRECTION('',(-1.,1.22464679914735E-16,-2.84598478402269E-15));
#4523=DIRECTION('',(-1.,1.22464679914735E-16,-2.84598478402269E-15));
#4524=DIRECTION('',(1.22464679914735E-16,1.,1.49975978266186E-32));
#4525=DIRECTION('',(1.,-1.22464679914735E-16,2.75774059927426E-15));
#4526=DIRECTION('',(1.22464679914735E-16,1.,1.49975978266186E-32));
#4527=DIRECTION('',(-1.,1.22464679914735E-16,-2.75774059927426E-15));
#4528=DIRECTION('',(-1.,1.22464679914735E-16,-2.84598478402269E-15));
#4529=DIRECTION('',(-1.,1.22464679914735E-16,-2.75774059927426E-15));
#4530=DIRECTION('',(1.,-1.22464679914735E-16,2.75774059927426E-15));
#4531=DIRECTION('',(-1.,1.22464679914735E-16,-2.84598478402269E-15));
#4532=DIRECTION('center_axis',(1.22464679914735E-16,1.,1.49975978266186E-32));
#4533=DIRECTION('ref_axis',(-0.707106824182888,8.65956108890821E-17,0.707106738190205));
#4534=DIRECTION('center_axis',(1.22464679914735E-16,1.,1.49975978266186E-32));
#4535=DIRECTION('ref_axis',(-0.707106824182888,8.65956108890821E-17,0.707106738190205));
#4536=DIRECTION('',(1.22464679914735E-16,1.,1.49975978266186E-32));
#4537=DIRECTION('center_axis',(-1.22464679914735E-16,-1.,-1.49975978266186E-32));
#4538=DIRECTION('ref_axis',(1.,-1.22464679914735E-16,1.22464679914735E-16));
#4539=DIRECTION('',(-1.,1.22464679914735E-16,-1.22464679914735E-16));
#4540=DIRECTION('',(1.22464679914735E-16,0.,-1.));
#4541=DIRECTION('',(-1.,1.22464679914735E-16,-2.68280906625521E-15));
#4542=DIRECTION('',(1.22464679914735E-16,0.,-1.));
#4543=DIRECTION('',(1.,-1.22464679914735E-16,1.22464679914735E-16));
#4544=DIRECTION('',(-1.,1.22464679914735E-16,-2.68280906625521E-15));
#4545=DIRECTION('center_axis',(-1.,1.22464679914735E-16,-1.22464679914735E-16));
#4546=DIRECTION('ref_axis',(1.22464679914735E-16,0.,-1.));
#4547=DIRECTION('',(1.22464679914735E-16,0.,-1.));
#4548=DIRECTION('',(-1.22464679914735E-16,-1.,-1.49975978266186E-32));
#4549=DIRECTION('center_axis',(1.22464679914735E-16,0.,-1.));
#4550=DIRECTION('ref_axis',(1.,-1.22464679914735E-16,1.22464679914735E-16));
#4551=DIRECTION('',(1.,-1.22464679914735E-16,1.22464679914735E-16));
#4552=DIRECTION('center_axis',(-1.,1.22464679914735E-16,-1.22464679914735E-16));
#4553=DIRECTION('ref_axis',(1.22464679914735E-16,0.,-1.));
#4554=DIRECTION('',(-1.22464679914735E-16,-1.,-1.49975978266186E-32));
#4555=DIRECTION('',(1.22464679914735E-16,0.,-1.));
#4556=DIRECTION('',(-1.22464679914735E-16,-1.,-1.49975978266186E-32));
#4557=DIRECTION('center_axis',(-1.,1.22464679914735E-16,-1.22464679914735E-16));
#4558=DIRECTION('ref_axis',(1.22464679914735E-16,0.,-1.));
#4559=DIRECTION('',(1.22464679914735E-16,0.,-1.));
#4560=DIRECTION('',(-1.1988727267528E-16,-0.999783049170591,-0.0208291764396907));
#4561=DIRECTION('',(1.22464679914735E-16,0.,-1.));
#4562=DIRECTION('',(5.16151446417155E-22,0.707108888531611,0.707104673835204));
#4563=DIRECTION('',(1.7319121124633E-16,0.707108888531611,-0.707104673835204));
#4564=DIRECTION('center_axis',(-1.22464679914735E-16,-1.,-1.49975978266186E-32));
#4565=DIRECTION('ref_axis',(1.22464679914735E-16,1.0252425757274E-46,-1.));
#4566=DIRECTION('',(1.22464679914735E-16,0.,-1.));
#4567=DIRECTION('center_axis',(-1.,1.22464679914735E-16,-1.22464679914735E-16));
#4568=DIRECTION('ref_axis',(1.22464679914735E-16,0.,-1.));
#4569=DIRECTION('',(1.22464679914735E-16,0.,-1.));
#4570=DIRECTION('',(-5.16151446417155E-22,-0.707108888531611,-0.707104673835204));
#4571=DIRECTION('',(-1.7319121124633E-16,-0.707108888531611,0.707104673835204));
#4572=DIRECTION('',(1.24988949526429E-16,0.999783049170591,-0.0208291764396907));
#4573=DIRECTION('center_axis',(1.22464679914735E-16,1.,1.49975978266186E-32));
#4574=DIRECTION('ref_axis',(1.22464679914735E-16,1.0252425757274E-46,-1.));
#4575=DIRECTION('',(-1.,1.22464679914735E-16,-1.22464679914735E-16));
#4576=DIRECTION('',(1.,-1.22464679914735E-16,1.22464679914735E-16));
#4577=DIRECTION('center_axis',(1.7319121124633E-16,0.707104673835204,-0.707108888531611));
#4578=DIRECTION('ref_axis',(-5.16151446399029E-22,-0.707108888531611,-0.707104673835204));
#4579=DIRECTION('',(-1.,1.22464679914735E-16,-1.22464679914735E-16));
#4580=DIRECTION('center_axis',(5.16151446417155E-22,-0.707104673835204,
-0.707108888531611));
#4581=DIRECTION('ref_axis',(-1.7319121124633E-16,-0.707108888531611,0.707104673835204));
#4582=DIRECTION('center_axis',(-1.1988727267528E-16,0.0208291764396907,
0.999783049170591));
#4583=DIRECTION('ref_axis',(1.24988949526429E-16,0.999783049170591,-0.0208291764396907));
#4584=DIRECTION('center_axis',(1.22464679914735E-16,1.,1.49975978266186E-32));
#4585=DIRECTION('ref_axis',(0.192330993613606,-2.35537535705732E-17,0.981330112090525));
#4586=DIRECTION('center_axis',(1.22464679914735E-16,1.,1.49975978266186E-32));
#4587=DIRECTION('ref_axis',(0.192330993613606,-2.35537535705732E-17,0.981330112090525));
#4588=DIRECTION('center_axis',(-1.22464679914735E-16,-1.,-1.49975978266186E-32));
#4589=DIRECTION('ref_axis',(0.192330993613606,-2.35537535705732E-17,0.981330112090525));
#4590=DIRECTION('center_axis',(1.22464679914735E-16,0.,-1.));
#4591=DIRECTION('ref_axis',(-1.,1.22464679914735E-16,-1.22464679914735E-16));
#4592=DIRECTION('',(-1.,1.22464679914735E-16,-1.22464679914735E-16));
#4593=DIRECTION('',(1.,-1.22464679914735E-16,1.22464679914735E-16));
#4594=DIRECTION('',(1.,-1.22464679914735E-16,1.22464679914735E-16));
#4595=DIRECTION('',(1.,-1.22464679914735E-16,1.22464679914735E-16));
#4596=DIRECTION('center_axis',(1.24988949526429E-16,0.0208291764396907,
-0.999783049170591));
#4597=DIRECTION('ref_axis',(-1.1988727267528E-16,-0.999783049170591,-0.0208291764396907));
#4598=DIRECTION('',(-1.,1.22464679914735E-16,-1.22464679914735E-16));
#4599=DIRECTION('center_axis',(1.22464679914735E-16,1.,1.49975978266186E-32));
#4600=DIRECTION('ref_axis',(1.22464679914735E-16,1.0252425757274E-46,-1.));
#4601=DIRECTION('',(1.,-1.22464679914735E-16,1.22464679914735E-16));
#4602=DIRECTION('center_axis',(-5.16151446417155E-22,0.707104673835204,
0.707108888531611));
#4603=DIRECTION('ref_axis',(1.7319121124633E-16,0.707108888531611,-0.707104673835204));
#4604=DIRECTION('',(-1.,1.22464679914735E-16,-1.22464679914735E-16));
#4605=DIRECTION('center_axis',(-1.7319121124633E-16,-0.707104673835204,
0.707108888531611));
#4606=DIRECTION('ref_axis',(5.16151446399029E-22,0.707108888531611,0.707104673835204));
#4607=DIRECTION('center_axis',(-1.22464679914735E-16,-1.,-1.49975978266186E-32));
#4608=DIRECTION('ref_axis',(1.22464679914735E-16,1.0252425757274E-46,-1.));
#4609=DIRECTION('',(-1.,1.22464679914735E-16,-1.22464679914735E-16));
#4610=DIRECTION('center_axis',(-1.22464679914735E-16,0.,1.));
#4611=DIRECTION('ref_axis',(-1.,1.22464679914735E-16,-1.22464679914735E-16));
#4612=DIRECTION('center_axis',(-1.,1.22464679914735E-16,-1.22464679914735E-16));
#4613=DIRECTION('ref_axis',(-1.22464679914735E-16,0.,1.));
#4614=DIRECTION('',(1.22464679914735E-16,0.,-1.));
#4615=DIRECTION('',(1.22464679914735E-16,1.,1.49975978266186E-32));
#4616=DIRECTION('',(1.7319121124633E-16,0.707108888531611,-0.707104673835204));
#4617=DIRECTION('',(1.22464679914735E-16,1.,0.));
#4618=DIRECTION('',(0.,-1.49975978266186E-32,1.));
#4619=DIRECTION('',(-1.22464679914735E-16,-1.,-1.49975978266186E-32));
#4620=DIRECTION('center_axis',(-1.,1.22464679914735E-16,-1.22464679914735E-16));
#4621=DIRECTION('ref_axis',(-1.22464679914735E-16,0.,1.));
#4622=DIRECTION('',(1.22464679914735E-16,0.,-1.));
#4623=DIRECTION('',(1.22464679914735E-16,1.,1.49975978266186E-32));
#4624=DIRECTION('',(0.,-1.49975978266186E-32,1.));
#4625=DIRECTION('',(-1.22464679914735E-16,-1.,0.));
#4626=DIRECTION('',(-6.28038757050967E-15,-0.707108888531611,-0.707104673835204));
#4627=DIRECTION('',(1.22464679914735E-16,1.,1.49975978266186E-32));
#4628=DIRECTION('center_axis',(-1.22464679914735E-16,0.,1.));
#4629=DIRECTION('ref_axis',(1.,-1.22464679914735E-16,1.22464679914735E-16));
#4630=DIRECTION('',(1.,-1.22464679914735E-16,2.77139240997905E-15));
#4631=DIRECTION('',(1.22464679914735E-16,1.,1.49975978266186E-32));
#4632=DIRECTION('',(1.22464679914735E-16,1.,1.49975978266186E-32));
#4633=DIRECTION('',(1.,-1.22464679914735E-16,1.22464679914735E-16));
#4634=DIRECTION('center_axis',(-1.22464679914735E-16,-1.,-1.49975978266186E-32));
#4635=DIRECTION('ref_axis',(1.,-1.22464679914735E-16,1.22464679914735E-16));
#4636=DIRECTION('center_axis',(1.22464679914735E-16,1.,1.49975978266186E-32));
#4637=DIRECTION('ref_axis',(1.,-1.22464679914735E-16,1.22464679914735E-16));
#4638=DIRECTION('center_axis',(1.22464679914735E-16,1.,1.49975978266186E-32));
#4639=DIRECTION('ref_axis',(1.,-1.22464679914735E-16,1.22464679914735E-16));
#4640=DIRECTION('',(1.22464679914735E-16,1.,1.49975978266186E-32));
#4641=DIRECTION('center_axis',(-1.22464679914735E-16,-1.,-1.49975978266186E-32));
#4642=DIRECTION('ref_axis',(1.,-1.22464679914735E-16,1.22464679914735E-16));
#4643=DIRECTION('center_axis',(2.76087478076931E-15,-3.23112048484961E-31,
-1.));
#4644=DIRECTION('ref_axis',(-1.,1.22464679914735E-16,-2.76087478076931E-15));
#4645=DIRECTION('',(1.,-1.22464679914735E-16,2.76087478076931E-15));
#4646=DIRECTION('',(1.22464679914735E-16,1.,1.49975978266186E-32));
#4647=DIRECTION('',(1.,-1.22464679914735E-16,4.87374585786276E-17));
#4648=DIRECTION('',(1.22464679914735E-16,1.,1.49975978266186E-32));
#4649=DIRECTION('',(-1.,1.22464679914735E-16,-4.87374585786276E-17));
#4650=DIRECTION('center_axis',(1.,-1.22464679914735E-16,1.22464679914735E-16));
#4651=DIRECTION('ref_axis',(1.22464679914735E-16,0.,-1.));
#4652=DIRECTION('',(-1.22464679914735E-16,0.,1.));
#4653=DIRECTION('',(1.22464679914735E-16,1.,1.49975978266186E-32));
#4654=DIRECTION('',(1.22464679914735E-16,0.,-1.));
#4655=DIRECTION('',(1.22464679914735E-16,1.,1.49975978266186E-32));
#4656=DIRECTION('center_axis',(1.22464679914735E-16,1.,1.49975978266186E-32));
#4657=DIRECTION('ref_axis',(-1.89882151931499E-15,2.17540971751502E-31,
1.));
#4658=DIRECTION('center_axis',(1.22464679914735E-16,1.,1.49975978266186E-32));
#4659=DIRECTION('ref_axis',(-1.89882151931499E-15,2.17540971751502E-31,
1.));
#4660=DIRECTION('center_axis',(-1.22464679914735E-16,-1.,-1.49975978266186E-32));
#4661=DIRECTION('ref_axis',(-1.89882151931499E-15,2.17540971751502E-31,
1.));
#4662=DIRECTION('center_axis',(1.22464679914735E-16,1.,1.49975978266186E-32));
#4663=DIRECTION('ref_axis',(-2.12086612424002E-15,2.4473359322044E-31,1.));
#4664=DIRECTION('center_axis',(-1.22464679914735E-16,-1.,-1.49975978266186E-32));
#4665=DIRECTION('ref_axis',(-2.12086612424002E-15,2.4473359322044E-31,1.));
#4666=DIRECTION('center_axis',(1.22464679914735E-16,1.,1.49975978266186E-32));
#4667=DIRECTION('ref_axis',(-2.12086612424002E-15,2.4473359322044E-31,1.));
#4668=DIRECTION('',(1.22464679914735E-16,1.,1.49975978266186E-32));
#4669=DIRECTION('center_axis',(-1.,1.22464679914735E-16,-1.22464679914735E-16));
#4670=DIRECTION('ref_axis',(-1.22464679914735E-16,0.,1.));
#4671=DIRECTION('',(-1.22464679914735E-16,0.,1.));
#4672=DIRECTION('',(-1.22464679914735E-16,0.,1.));
#4673=DIRECTION('',(1.22464679914735E-16,1.,1.49975978266186E-32));
#4674=DIRECTION('center_axis',(0.,0.,-1.));
#4675=DIRECTION('ref_axis',(-1.22464679914735E-16,-1.,0.));
#4676=DIRECTION('',(-1.,1.22464679914735E-16,0.));
#4677=DIRECTION('',(1.22464679914735E-16,1.,0.));
#4678=DIRECTION('',(1.,0.,0.));
#4679=DIRECTION('center_axis',(0.,0.707104673835204,-0.707108888531611));
#4680=DIRECTION('ref_axis',(-6.28038757050967E-15,-0.707108888531611,-0.707104673835204));
#4681=DIRECTION('',(6.28038757050967E-15,0.707108888531611,0.707104673835204));
#4682=DIRECTION('',(1.,1.22465409865287E-16,1.22464679914735E-16));
#4683=DIRECTION('center_axis',(0.,0.707104673835204,0.707108888531611));
#4684=DIRECTION('ref_axis',(1.7319121124633E-16,0.707108888531611,-0.707104673835204));
#4685=DIRECTION('',(-1.,1.22465409865287E-16,-1.22464679914735E-16));
#4686=DIRECTION('',(-1.7319121124633E-16,-0.707108888531611,0.707104673835204));
#4687=DIRECTION('',(-1.,0.,0.));
#4688=DIRECTION('center_axis',(0.,0.,1.));
#4689=DIRECTION('ref_axis',(1.22464679914735E-16,1.,0.));
#4690=DIRECTION('',(-1.22464679914735E-16,-1.,0.));
#4691=DIRECTION('',(1.,-1.22464679914735E-16,0.));
#4692=DIRECTION('center_axis',(-1.22464679914735E-16,-1.,-1.49975978266186E-32));
#4693=DIRECTION('ref_axis',(1.,-1.22464679914735E-16,1.22464679914735E-16));
#4694=DIRECTION('',(0.707106606671929,-8.65955842516724E-17,0.707106955701123));
#4695=DIRECTION('center_axis',(-1.22464679914735E-16,-1.,-1.49975978266186E-32));
#4696=DIRECTION('ref_axis',(0.707106824182887,-8.65956108890821E-17,-0.707106738190205));
#4697=DIRECTION('',(1.,-1.22464679914735E-16,1.22464679914735E-16));
#4698=DIRECTION('',(0.,1.49975978266186E-32,-1.));
#4699=DIRECTION('center_axis',(-1.22464679914735E-16,-1.,-1.49975978266186E-32));
#4700=DIRECTION('ref_axis',(-0.192330993613605,2.35537535705731E-17,-0.981330112090526));
#4701=DIRECTION('',(0.797940776019378,-9.77195617261287E-17,0.602735860859127));
#4702=DIRECTION('center_axis',(-1.22464679914735E-16,-1.,-1.49975978266186E-32));
#4703=DIRECTION('ref_axis',(0.619814087082361,-7.5905333781185E-17,-0.784748684264115));
#4704=DIRECTION('',(1.22464679914735E-16,0.,-1.));
#4705=DIRECTION('center_axis',(-1.22464679914735E-16,-1.,-1.49975978266186E-32));
#4706=DIRECTION('ref_axis',(0.70710688994201,-8.6595618942252E-17,-0.707106672431068));
#4707=DIRECTION('',(0.707106672431068,-8.65955923048443E-17,0.707106889942011));
#4708=DIRECTION('',(1.22464679914735E-16,0.,-1.));
#4709=DIRECTION('',(1.,-1.22464679914735E-16,2.76087478076931E-15));
#4710=DIRECTION('center_axis',(1.22464679914735E-16,1.,1.49975978266186E-32));
#4711=DIRECTION('ref_axis',(0.999999975140088,-1.22464676870274E-16,-0.000222979425697547));
#4712=DIRECTION('',(-0.000222979425718486,2.73071039982009E-20,-0.999999975140088));
#4713=DIRECTION('center_axis',(1.22464679914735E-16,1.,1.49975978266186E-32));
#4714=DIRECTION('ref_axis',(-0.149925588670012,1.83605892275013E-17,-0.988697283227758));
#4715=DIRECTION('center_axis',(-1.22464679914735E-16,0.,1.));
#4716=DIRECTION('ref_axis',(1.,-1.22464679914735E-16,1.22464679914735E-16));
#4717=DIRECTION('',(-1.,1.22464679914735E-16,-1.22464679914735E-16));
#4718=DIRECTION('',(1.22464679914735E-16,1.,1.49975978266186E-32));
#4719=DIRECTION('center_axis',(-1.22464679914735E-16,-1.,-1.49975978266186E-32));
#4720=DIRECTION('ref_axis',(1.,-1.22464679914735E-16,1.22464679914735E-16));
#4721=DIRECTION('',(1.,-1.22464679914735E-16,1.22464679914735E-16));
#4722=DIRECTION('',(-1.22464679914735E-16,0.,1.));
#4723=DIRECTION('',(1.,-1.22464679914735E-16,2.77139240997905E-15));
#4724=DIRECTION('center_axis',(1.22464679914735E-16,1.,1.49975978266186E-32));
#4725=DIRECTION('ref_axis',(0.707106824182887,-8.65956108890821E-17,-0.707106738190205));
#4726=DIRECTION('',(-1.,1.22464679914735E-16,-4.87374585786276E-17));
#4727=DIRECTION('',(-1.22464679914735E-16,0.,1.));
#4728=DIRECTION('center_axis',(0.707106955701123,-8.6595626995421E-17,-0.707106606671929));
#4729=DIRECTION('ref_axis',(-0.707106606671929,8.65955842516724E-17,-0.707106955701123));
#4730=DIRECTION('',(-0.707106606671929,8.65955842516724E-17,-0.707106955701123));
#4731=DIRECTION('',(1.22464679914735E-16,1.,1.49975978266186E-32));
#4732=DIRECTION('center_axis',(1.22464679914735E-16,1.,1.49975978266186E-32));
#4733=DIRECTION('ref_axis',(-0.192330993613605,2.35537535705731E-17,-0.981330112090526));
#4734=DIRECTION('center_axis',(1.22464679914735E-16,1.,1.49975978266186E-32));
#4735=DIRECTION('ref_axis',(-0.192330993613605,2.35537535705731E-17,-0.981330112090526));
#4736=DIRECTION('',(1.22464679914735E-16,1.,1.49975978266186E-32));
#4737=DIRECTION('center_axis',(-1.22464679914735E-16,-1.,-1.49975978266186E-32));
#4738=DIRECTION('ref_axis',(1.,-1.22464679914735E-16,1.22464679914735E-16));
#4739=DIRECTION('',(0.707106672431068,-8.65955923048443E-17,0.707106889942011));
#4740=DIRECTION('center_axis',(-1.22464679914735E-16,-1.,-1.49975978266186E-32));
#4741=DIRECTION('ref_axis',(0.70710688994201,-8.6595618942252E-17,-0.707106672431068));
#4742=DIRECTION('',(1.22464679914735E-16,0.,-1.));
#4743=DIRECTION('center_axis',(1.22464679914735E-16,1.,1.49975978266186E-32));
#4744=DIRECTION('ref_axis',(0.619814087082361,-7.5905333781185E-17,-0.784748684264115));
#4745=DIRECTION('',(-0.797940776019378,9.77195617261287E-17,-0.602735860859127));
#4746=DIRECTION('center_axis',(-1.22464679914735E-16,-1.,-1.49975978266186E-32));
#4747=DIRECTION('ref_axis',(-0.149925588670012,1.83605892275013E-17,-0.988697283227758));
#4748=DIRECTION('',(0.000222979425718486,-2.73071039982009E-20,0.999999975140088));
#4749=DIRECTION('center_axis',(-1.22464679914735E-16,-1.,-1.49975978266186E-32));
#4750=DIRECTION('ref_axis',(0.999999975140088,-1.22464676870274E-16,-0.000222979425697547));
#4751=DIRECTION('',(1.,-1.22464679914735E-16,4.87374585786276E-17));
#4752=DIRECTION('center_axis',(1.22464679914735E-16,1.,1.49975978266186E-32));
#4753=DIRECTION('ref_axis',(0.707106824182887,-8.65956108890821E-17,-0.707106738190205));
#4754=DIRECTION('center_axis',(1.,-1.22464679914735E-16,1.22464679914735E-16));
#4755=DIRECTION('ref_axis',(1.22464679914735E-16,0.,-1.));
#4756=DIRECTION('',(1.22464679914735E-16,1.,1.49975978266186E-32));
#4757=DIRECTION('center_axis',(1.22464679914735E-16,0.,-1.));
#4758=DIRECTION('ref_axis',(-1.,1.22464679914735E-16,-1.22464679914735E-16));
#4759=DIRECTION('',(1.22464679914735E-16,1.,1.49975978266186E-32));
#4760=DIRECTION('center_axis',(1.,-1.22464679914735E-16,1.22464679914735E-16));
#4761=DIRECTION('ref_axis',(1.22464679914735E-16,0.,-1.));
#4762=DIRECTION('',(-1.22464679914735E-16,-1.,-1.49975978266186E-32));
#4763=DIRECTION('center_axis',(2.76087478076931E-15,-3.23112048484961E-31,
-1.));
#4764=DIRECTION('ref_axis',(-1.,1.22464679914735E-16,-2.76087478076931E-15));
#4765=DIRECTION('',(1.22464679914735E-16,1.,1.49975978266186E-32));
#4766=DIRECTION('',(1.22464679914735E-16,1.,1.49975978266186E-32));
#4767=DIRECTION('center_axis',(1.22464679914735E-16,1.,1.49975978266186E-32));
#4768=DIRECTION('ref_axis',(0.999999975140088,-1.22464676870274E-16,-0.000222979425697547));
#4769=DIRECTION('',(1.22464679914735E-16,1.,1.49975978266186E-32));
#4770=DIRECTION('center_axis',(-0.999999975140088,1.22464676870274E-16,
0.000222979425718486));
#4771=DIRECTION('ref_axis',(0.000222979425718486,-2.73071039982009E-20,
0.999999975140088));
#4772=DIRECTION('',(1.22464679914735E-16,1.,1.49975978266186E-32));
#4773=DIRECTION('center_axis',(1.22464679914735E-16,1.,1.49975978266186E-32));
#4774=DIRECTION('ref_axis',(-0.149925588670012,1.83605892275013E-17,-0.988697283227758));
#4775=DIRECTION('center_axis',(0.602735860859127,-7.38138542732454E-17,
-0.797940776019378));
#4776=DIRECTION('ref_axis',(-0.797940776019378,9.77195617261287E-17,-0.602735860859127));
#4777=DIRECTION('',(1.22464679914735E-16,1.,1.49975978266186E-32));
#4778=DIRECTION('center_axis',(1.22464679914735E-16,1.,1.49975978266186E-32));
#4779=DIRECTION('ref_axis',(0.619814087082361,-7.5905333781185E-17,-0.784748684264115));
#4780=DIRECTION('',(1.22464679914735E-16,1.,1.49975978266186E-32));
#4781=DIRECTION('center_axis',(1.,-1.22464679914735E-16,1.22464679914735E-16));
#4782=DIRECTION('ref_axis',(1.22464679914735E-16,0.,-1.));
#4783=DIRECTION('',(1.22464679914735E-16,1.,1.49975978266186E-32));
#4784=DIRECTION('center_axis',(1.22464679914735E-16,1.,1.49975978266186E-32));
#4785=DIRECTION('ref_axis',(0.382683511888619,-4.68652137920864E-17,0.923879499571558));
#4786=DIRECTION('',(-1.22464679914735E-16,-1.,-1.49975978266186E-32));
#4787=DIRECTION('center_axis',(-1.22464679914735E-16,0.,1.));
#4788=DIRECTION('ref_axis',(1.,-1.22464679914735E-16,1.22464679914735E-16));
#4789=DIRECTION('',(1.22464679914735E-16,1.,1.49975978266186E-32));
#4790=DIRECTION('',(1.22464679914735E-16,1.,1.49975978266186E-32));
#4791=DIRECTION('center_axis',(1.22464679914735E-16,1.,1.49975978266186E-32));
#4792=DIRECTION('ref_axis',(0.707106824182887,-8.65956108890821E-17,-0.707106738190205));
#4793=DIRECTION('center_axis',(-0.707106889942011,8.65956189422523E-17,
0.707106672431068));
#4794=DIRECTION('ref_axis',(0.707106672431068,-8.65955923048443E-17,0.707106889942011));
#4795=DIRECTION('axis',(0.,0.,1.));
#4796=DIRECTION('refdir',(1.,0.,0.));
#4797=DIRECTION('center_axis',(0.,-1.,0.));
#4798=DIRECTION('ref_axis',(1.,0.,0.));
#4799=DIRECTION('center_axis',(0.,1.,0.));
#4800=DIRECTION('ref_axis',(1.,0.,0.));
#4801=DIRECTION('center_axis',(0.,-1.,0.));
#4802=DIRECTION('ref_axis',(1.,0.,0.));
#4803=DIRECTION('center_axis',(0.,-1.,0.));
#4804=DIRECTION('ref_axis',(1.,0.,0.));
#4805=DIRECTION('',(0.,1.,0.));
#4806=DIRECTION('center_axis',(0.,-1.,0.));
#4807=DIRECTION('ref_axis',(1.,0.,0.));
#4808=DIRECTION('axis',(0.,0.,1.));
#4809=DIRECTION('refdir',(1.,0.,0.));
#4810=DIRECTION('center_axis',(0.,-1.,0.));
#4811=DIRECTION('ref_axis',(-1.,0.,0.));
#4812=DIRECTION('center_axis',(1.83667601732677E-48,-1.,2.24927940568994E-64));
#4813=DIRECTION('ref_axis',(-1.,-1.83667601732677E-48,0.));
#4814=DIRECTION('',(0.,1.,0.));
#4815=DIRECTION('center_axis',(-1.83667601732677E-48,1.,-2.24927940568994E-64));
#4816=DIRECTION('ref_axis',(-1.,-1.83667601732677E-48,0.));
#4817=DIRECTION('center_axis',(-1.83667601732677E-48,1.,-2.24927940568994E-64));
#4818=DIRECTION('ref_axis',(-1.,-1.83667601732677E-48,0.));
#4819=DIRECTION('center_axis',(-1.83667601732677E-48,1.,-2.24927940568994E-64));
#4820=DIRECTION('ref_axis',(-1.,-1.83667601732677E-48,0.));
#4821=DIRECTION('axis',(0.,0.,1.));
#4822=DIRECTION('refdir',(1.,0.,0.));
#4823=DIRECTION('center_axis',(0.,-1.,0.));
#4824=DIRECTION('ref_axis',(-1.,0.,0.));
#4825=DIRECTION('center_axis',(1.83667601732677E-48,-1.,2.73691106313441E-48));
#4826=DIRECTION('ref_axis',(-1.,-1.83667601732677E-48,0.));
#4827=DIRECTION('',(0.,1.,0.));
#4828=DIRECTION('center_axis',(-1.83667601732677E-48,1.,-2.73691106313441E-48));
#4829=DIRECTION('ref_axis',(-1.,-1.83667601732677E-48,0.));
#4830=DIRECTION('center_axis',(-1.83667601732677E-48,1.,-2.73691106313441E-48));
#4831=DIRECTION('ref_axis',(-1.,-1.83667601732677E-48,0.));
#4832=DIRECTION('center_axis',(-1.83667601732677E-48,1.,-2.73691106313441E-48));
#4833=DIRECTION('ref_axis',(-1.,-1.83667601732677E-48,0.));
#4834=DIRECTION('axis',(0.,0.,1.));
#4835=DIRECTION('refdir',(1.,0.,0.));
#4836=DIRECTION('center_axis',(0.,0.0208291764396898,-0.999783049170591));
#4837=DIRECTION('ref_axis',(1.,0.,0.));
#4838=DIRECTION('center_axis',(0.,0.0208291764396898,-0.999783049170591));
#4839=DIRECTION('ref_axis',(1.,0.,0.));
#4840=DIRECTION('',(0.,-0.0208291764396898,0.999783049170591));
#4841=DIRECTION('center_axis',(0.,-0.0208291764396898,0.999783049170591));
#4842=DIRECTION('ref_axis',(1.,0.,0.));
#4843=DIRECTION('center_axis',(0.,-0.0208291764396898,0.999783049170591));
#4844=DIRECTION('ref_axis',(1.,0.,0.));
#4845=DIRECTION('center_axis',(0.,-0.0208291764396898,0.999783049170591));
#4846=DIRECTION('ref_axis',(1.,0.,0.));
#4847=DIRECTION('axis',(0.,0.,1.));
#4848=DIRECTION('refdir',(1.,0.,0.));
#4849=DIRECTION('center_axis',(0.,-1.,0.));
#4850=DIRECTION('ref_axis',(1.,0.,0.));
#4851=DIRECTION('center_axis',(0.,1.,0.));
#4852=DIRECTION('ref_axis',(1.,0.,0.));
#4853=DIRECTION('center_axis',(0.,-1.,0.));
#4854=DIRECTION('ref_axis',(1.,0.,0.));
#4855=DIRECTION('center_axis',(0.,-1.,0.));
#4856=DIRECTION('ref_axis',(1.,0.,0.));
#4857=DIRECTION('',(0.,1.,0.));
#4858=DIRECTION('center_axis',(0.,-1.,0.));
#4859=DIRECTION('ref_axis',(1.,0.,0.));
#4860=DIRECTION('axis',(0.,0.,1.));
#4861=DIRECTION('refdir',(1.,0.,0.));
#4862=DIRECTION('center_axis',(2.44876222201709E-16,-0.0208291764396898,
-0.999783049170591));
#4863=DIRECTION('ref_axis',(1.,-7.39048179408127E-33,2.44929359829471E-16));
#4864=DIRECTION('center_axis',(-2.44876222201709E-16,0.0208291764396898,
0.999783049170591));
#4865=DIRECTION('ref_axis',(1.,-7.39048179408127E-33,2.44929359829471E-16));
#4866=DIRECTION('',(-2.44876222201709E-16,0.0208291764396898,0.999783049170591));
#4867=DIRECTION('center_axis',(2.44876222201709E-16,-0.0208291764396898,
-0.999783049170591));
#4868=DIRECTION('ref_axis',(1.,-7.39048179408127E-33,2.44929359829471E-16));
#4869=DIRECTION('center_axis',(-2.44876222201709E-16,0.0208291764396898,
0.999783049170591));
#4870=DIRECTION('ref_axis',(1.,-7.39048179408127E-33,2.44929359829471E-16));
#4871=DIRECTION('center_axis',(-2.44876222201709E-16,0.0208291764396898,
0.999783049170591));
#4872=DIRECTION('ref_axis',(1.,-7.39048179408127E-33,2.44929359829471E-16));
#4873=DIRECTION('',(0.,0.,1.));
#4874=DIRECTION('',(1.,0.,0.));
#4875=DIRECTION('',(0.,0.,1.));
#4876=DIRECTION('',(1.,0.,0.));
#4877=DIRECTION('',(0.,0.,1.));
#4878=DIRECTION('',(1.,0.,0.));
#4879=DIRECTION('',(0.,0.,1.));
#4880=DIRECTION('',(1.,0.,0.));
#4881=DIRECTION('',(0.,0.,1.));
#4882=DIRECTION('',(1.,0.,0.));
#4883=DIRECTION('',(0.,0.,1.));
#4884=DIRECTION('',(1.,0.,0.));
#4885=DIRECTION('',(0.,0.,1.));
#4886=DIRECTION('',(1.,0.,0.));
#4887=DIRECTION('',(0.,0.,1.));
#4888=DIRECTION('',(1.,0.,0.));
#4889=CARTESIAN_POINT('',(0.,0.,0.));
#4890=CARTESIAN_POINT('',(0.,0.,0.));
#4891=CARTESIAN_POINT('Origin',(55.4902124404907,-11.9018738839031,101.14418999359));
#4892=CARTESIAN_POINT('',(56.823388803725,-10.4113449571108,101.175243220618));
#4893=CARTESIAN_POINT('',(54.1570360772564,-10.4113449571108,101.175243220618));
#4894=CARTESIAN_POINT('',(55.4902124404907,-10.4113449571108,101.175243220618));
#4895=CARTESIAN_POINT('Origin',(55.4902124404907,-11.9018738839031,101.14418999359));
#4896=CARTESIAN_POINT('Origin',(55.4902124404907,-12.0000001341105,105.854167938232));
#4897=CARTESIAN_POINT('',(53.4902124404907,-11.9197037286391,102.000007629395));
#4898=CARTESIAN_POINT('Origin',(55.4902124404907,-11.9197037286391,102.000007629395));
#4899=CARTESIAN_POINT('',(53.4902124404907,-11.9031683527619,101.206323416217));
#4900=CARTESIAN_POINT('',(53.4902124404907,-12.0000001341105,105.854167938232));
#4901=CARTESIAN_POINT('Origin',(55.4902124404907,-11.9031683527619,101.206323416217));
#4902=CARTESIAN_POINT('Origin',(55.4902124404907,-11.9031683527619,101.206323416217));
#4903=CARTESIAN_POINT('Origin',(55.4902124404907,-12.0000001341105,105.854167938232));
#4904=CARTESIAN_POINT('',(53.4902124404907,-11.998698570337,105.791693965635));
#4905=CARTESIAN_POINT('Origin',(55.4902124404907,-11.998698570337,105.791693965635));
#4906=CARTESIAN_POINT('',(53.4902124404907,-11.9822046586727,105.));
#4907=CARTESIAN_POINT('',(53.4902124404907,-12.0000001341105,105.854167938232));
#4908=CARTESIAN_POINT('Origin',(55.4902124404907,-11.9822046586727,105.));
#4909=CARTESIAN_POINT('Origin',(55.4902124404907,-4.00000013411045,0.145828066207017));
#4910=CARTESIAN_POINT('',(55.5312016298222,-1.92132882178138,3.92132133245468));
#4911=CARTESIAN_POINT('',(53.4902124404907,-3.92134265391535,3.92132133245468));
#4912=CARTESIAN_POINT('Origin',(55.4902124404907,-3.92134265391535,3.92132133245468));
#4913=CARTESIAN_POINT('',(55.4492232511593,-1.92132882178138,3.92132133245468));
#4914=CARTESIAN_POINT('Origin',(55.4902124404907,-3.88052558675829,5.88050641971165));
#4915=CARTESIAN_POINT('Origin',(55.4902124404907,-3.92134265391535,3.92132133245468));
#4916=CARTESIAN_POINT('',(53.4902124404907,-3.97803783517153,1.20000004768372));
#4917=CARTESIAN_POINT('',(53.4902124404907,-4.00000013411045,0.145828066207016));
#4918=CARTESIAN_POINT('Origin',(55.4902124404907,-3.97803783517153,1.20000004768372));
#4919=CARTESIAN_POINT('Origin',(50.4902124404907,0.,3.92132133245468));
#4920=CARTESIAN_POINT('',(50.4902111949968,-1.92132882178138,3.92132133245468));
#4921=CARTESIAN_POINT('',(52.9902111948072,-1.92132882178138,3.92132133245468));
#4922=CARTESIAN_POINT('',(50.4902124404907,-8.,3.92132133245468));
#4923=CARTESIAN_POINT('',(50.4902124404907,0.,3.92132133245468));
#4924=CARTESIAN_POINT('',(60.4902124404907,-8.,3.92132133245468));
#4925=CARTESIAN_POINT('',(51.5279682097109,-8.,3.92132133245468));
#4926=CARTESIAN_POINT('',(60.4902111949968,-1.92132882178138,3.92132133245468));
#4927=CARTESIAN_POINT('',(60.4902124404907,0.,3.92132133245468));
#4928=CARTESIAN_POINT('',(52.9902111948072,-1.92132882178138,3.92132133245468));
#4929=CARTESIAN_POINT('Origin',(10.0000045479708,-8.,103.499999046326));
#4930=CARTESIAN_POINT('',(8.50000441279955,-8.,103.499999046326));
#4931=CARTESIAN_POINT('Origin',(10.0000045479708,-8.,103.499999046326));
#4932=CARTESIAN_POINT('',(8.50000441279955,-2.8,103.499999046326));
#4933=CARTESIAN_POINT('',(8.50000441279957,-8.,103.499999046326));
#4934=CARTESIAN_POINT('Origin',(10.0000045479708,-2.8,103.499999046326));
#4935=CARTESIAN_POINT('Origin',(10.0000045479708,-2.8,103.499999046326));
#4936=CARTESIAN_POINT('Origin',(100.979996788778,-8.,2.49999516053467));
#4937=CARTESIAN_POINT('',(99.4799971640107,-8.,2.49999516053467));
#4938=CARTESIAN_POINT('Origin',(100.979996788778,-8.,2.49999516053467));
#4939=CARTESIAN_POINT('',(99.4799971640107,-2.8,2.49999516053467));
#4940=CARTESIAN_POINT('',(99.4799971640111,-8.,2.49999516053467));
#4941=CARTESIAN_POINT('Origin',(100.979996788778,-2.8,2.49999516053467));
#4942=CARTESIAN_POINT('Origin',(100.979996788778,-2.8,2.49999516053467));
#4943=CARTESIAN_POINT('Origin',(50.4902124404907,0.,4.99999999999986));
#4944=CARTESIAN_POINT('',(50.4902124404907,-8.,4.99999999999986));
#4945=CARTESIAN_POINT('',(50.4902124404907,-8.,3.74999999999986));
#4946=CARTESIAN_POINT('',(50.4902099495032,-1.00000000000001,2.99999800221971));
#4947=CARTESIAN_POINT('',(50.4902099491237,-1.00000000000001,2.99999800221971));
#4948=CARTESIAN_POINT('',(50.4902099495032,0.,2.99999800221971));
#4949=CARTESIAN_POINT('',(50.4902099491237,-1.00000000000001,2.99999800221971));
#4950=CARTESIAN_POINT('',(50.4902111949971,0.,4.99999999999986));
#4951=CARTESIAN_POINT('',(50.4902099491237,0.,28.230330787343));
#4952=CARTESIAN_POINT('',(50.4902124404907,0.,4.99999999999986));
#4953=CARTESIAN_POINT('Origin',(50.4902124404907,0.,1.20000004768372));
#4954=CARTESIAN_POINT('',(50.4902124404907,-8.,-1.59733337667944E-13));
#4955=CARTESIAN_POINT('',(50.4902124404907,-8.,1.20000004768372));
#4956=CARTESIAN_POINT('',(50.4902124404907,-8.,1.85000002384179));
#4957=CARTESIAN_POINT('',(50.4902111949971,0.,0.));
#4958=CARTESIAN_POINT('',(50.4902124404907,0.,0.));
#4959=CARTESIAN_POINT('',(50.4902099495032,0.,1.99999418752244));
#4960=CARTESIAN_POINT('',(50.4902099491237,0.,27.2999995124759));
#4961=CARTESIAN_POINT('',(50.4902099495032,-1.00000000000001,1.99999418752245));
#4962=CARTESIAN_POINT('',(50.4902099491237,1.73686967253925,1.99999418752245));
#4963=CARTESIAN_POINT('',(50.4902111949968,-1.79999890820268,1.20000004768372));
#4964=CARTESIAN_POINT('',(50.4902099491237,-2.00000023841859,0.999999909568344));
#4965=CARTESIAN_POINT('',(50.4902124404907,0.,1.20000004768372));
#4966=CARTESIAN_POINT('Origin',(5.0000011920929,0.,0.));
#4967=CARTESIAN_POINT('',(5.,-8.,-1.27675647831893E-14));
#4968=CARTESIAN_POINT('',(5.,-8.,-1.27675647831893E-14));
#4969=CARTESIAN_POINT('',(5.00000059604645,-7.,-6.38378239159465E-15));
#4970=CARTESIAN_POINT('',(5.,0.,-1.27675647831893E-14));
#4971=CARTESIAN_POINT('',(5.0000011920929,0.,0.));
#4972=CARTESIAN_POINT('',(5.0000011920929,0.,0.));
#4973=CARTESIAN_POINT('',(0.,0.,0.));
#4974=CARTESIAN_POINT('Origin',(10.0000020566037,-2.8,2.50000086324266));
#4975=CARTESIAN_POINT('',(8.25000236106051,-2.8,2.50000086324266));
#4976=CARTESIAN_POINT('Origin',(10.0000020566037,-2.8,2.50000086324266));
#4977=CARTESIAN_POINT('Origin',(10.0000020566037,0.,2.50000086324266));
#4978=CARTESIAN_POINT('',(8.25000236106051,-8.,2.50000086324266));
#4979=CARTESIAN_POINT('',(8.25000236106046,0.,2.50000086324266));
#4980=CARTESIAN_POINT('Origin',(10.0000020566037,-8.,2.50000086324266));
#4981=CARTESIAN_POINT('Origin',(75.2228282332459,0.,4.9999999999998));
#4982=CARTESIAN_POINT('',(9.99999999999999,0.,4.99999999999997));
#4983=CARTESIAN_POINT('',(9.99999999999999,0.,4.99999999999997));
#4984=CARTESIAN_POINT('',(9.99999999999999,-7.,4.99999999999997));
#4985=CARTESIAN_POINT('',(9.99999999999999,0.,4.99999999999997));
#4986=CARTESIAN_POINT('',(5.55111512312579E-15,-7.,5.00000039726821));
#4987=CARTESIAN_POINT('',(79.9288641879263,-7.,5.00000000000001));
#4988=CARTESIAN_POINT('',(1.33226762955019E-14,-8.,5.));
#4989=CARTESIAN_POINT('',(1.33226762955019E-14,0.,5.));
#4990=CARTESIAN_POINT('',(1.33226762955019E-14,-8.,5.));
#4991=CARTESIAN_POINT('Origin',(5.00000000000001,0.,9.99999999999997));
#4992=CARTESIAN_POINT('',(5.00000000000001,0.,40.7547938331316));
#4993=CARTESIAN_POINT('',(5.00000000000001,0.,9.99999999999997));
#4994=CARTESIAN_POINT('',(5.00000000000001,0.,9.99999999999997));
#4995=CARTESIAN_POINT('',(5.00000000000001,-7.,40.7547938331316));
#4996=CARTESIAN_POINT('',(5.00000000000001,0.,40.7547938331316));
#4997=CARTESIAN_POINT('',(5.00000000000001,-7.,9.99999999999997));
#4998=CARTESIAN_POINT('',(5.00000000000001,-7.,9.99999999999997));
#4999=CARTESIAN_POINT('',(5.00000000000001,0.,9.99999999999997));
#5000=CARTESIAN_POINT('Origin',(10.,0.,9.99999999999996));
#5001=CARTESIAN_POINT('Origin',(10.,0.,9.99999999999996));
#5002=CARTESIAN_POINT('Origin',(10.,-7.,9.99999999999996));
#5003=CARTESIAN_POINT('Origin',(5.00000000000001,0.,4.99999999999998));
#5004=CARTESIAN_POINT('',(0.,0.,5.0000011920929));
#5005=CARTESIAN_POINT('Origin',(5.00000000000001,0.,4.99999999999998));
#5006=CARTESIAN_POINT('Origin',(5.00000000000001,-8.,4.99999999999998));
#5007=CARTESIAN_POINT('',(0.,0.,5.0000011920929));
#5008=CARTESIAN_POINT('Origin',(0.,0.,44.9598550796509));
#5009=CARTESIAN_POINT('',(0.,0.,44.9598550796509));
#5010=CARTESIAN_POINT('',(0.,0.,106.000003814697));
#5011=CARTESIAN_POINT('',(0.,-7.,44.9598550796509));
#5012=CARTESIAN_POINT('',(0.,-7.,106.000003814697));
#5013=CARTESIAN_POINT('',(0.,0.,44.9598550796509));
#5014=CARTESIAN_POINT('Origin',(55.4902099491237,-1.00000000000001,1.99999418752245));
#5015=CARTESIAN_POINT('',(60.4902099495032,-2.77555756156289E-16,1.99999418752245));
#5016=CARTESIAN_POINT('',(55.4902111948072,0.,1.99999418752244));
#5017=CARTESIAN_POINT('',(60.4902099495032,-1.00000000000001,1.99999418752245));
#5018=CARTESIAN_POINT('',(60.4902099491237,1.73686967253925,1.99999418752245));
#5019=CARTESIAN_POINT('',(55.4902099491237,-1.00000000000001,1.99999418752245));
#5020=CARTESIAN_POINT('Origin',(55.4902099491237,-1.79999890820268,1.20000004768372));
#5021=CARTESIAN_POINT('',(60.4902111949968,-1.79999890820268,1.20000004768372));
#5022=CARTESIAN_POINT('',(60.4902099491237,-2.00000023841859,0.999999909568345));
#5023=CARTESIAN_POINT('',(57.9902111948072,-1.79999890820268,1.20000004768372));
#5024=CARTESIAN_POINT('Origin',(55.4902099491237,-1.00000000000001,2.99999800221971));
#5025=CARTESIAN_POINT('',(60.4902099495032,-1.00000000000001,2.99999800221971));
#5026=CARTESIAN_POINT('',(60.4902099491237,-1.00000000000001,2.99999800221971));
#5027=CARTESIAN_POINT('',(55.4902099491237,-1.00000000000001,2.99999800221971));
#5028=CARTESIAN_POINT('Origin',(55.4902099491237,-1.38777878078145E-16,
2.99999800221971));
#5029=CARTESIAN_POINT('',(60.4902111949968,-1.85037170770859E-16,2.99999800221971));
#5030=CARTESIAN_POINT('',(60.4902099491237,-1.00000000000001,2.99999800221971));
#5031=CARTESIAN_POINT('',(55.4902111948072,0.,2.99999800221971));
#5032=CARTESIAN_POINT('Origin',(52.5657239789312,-8.,2.49999999999987));
#5033=CARTESIAN_POINT('',(60.4902124404907,-8.,1.20000004768372));
#5034=CARTESIAN_POINT('',(56.5279682097109,-8.,1.20000004768372));
#5035=CARTESIAN_POINT('',(60.4902124404907,-8.,-1.59733337667944E-13));
#5036=CARTESIAN_POINT('',(60.4902124404907,-8.,1.24999999999985));
#5037=CARTESIAN_POINT('',(102.131447957862,-8.,-2.70061750740069E-13));
#5038=CARTESIAN_POINT('',(5.,-8.,-1.27675647831893E-14));
#5039=CARTESIAN_POINT('',(104.367515935362,-8.,5.));
#5040=CARTESIAN_POINT('Origin',(102.131447957862,-8.,2.99999999999972));
#5041=CARTESIAN_POINT('',(60.4902124404907,-8.,4.99999999999983));
#5042=CARTESIAN_POINT('',(1.33226762955019E-14,-8.,5.));
#5043=CARTESIAN_POINT('',(60.4902124404907,-8.,3.21066066622727));
#5044=CARTESIAN_POINT('Origin',(19.277690708776,0.,-53.4006744879114));
#5045=CARTESIAN_POINT('',(78.0377025773334,-7.,27.8008288299553));
#5046=CARTESIAN_POINT('Origin',(19.277690708776,-7.,-53.4006744879114));
#5047=CARTESIAN_POINT('',(78.0377025773334,0.,27.8008288299553));
#5048=CARTESIAN_POINT('',(78.0377025773334,0.,27.8008288299553));
#5049=CARTESIAN_POINT('Origin',(19.277690708776,0.,-53.4006744879114));
#5050=CARTESIAN_POINT('Origin',(60.4902124404907,0.,3.92132133245468));
#5051=CARTESIAN_POINT('',(60.4902124404907,0.,4.99999999999983));
#5052=CARTESIAN_POINT('',(60.4902124404907,0.,4.99999999999984));
#5053=CARTESIAN_POINT('',(60.4902124404907,0.,28.4606616199017));
#5054=CARTESIAN_POINT('Origin',(60.4902124404907,0.,1.20000004768372));
#5055=CARTESIAN_POINT('',(60.4902124404907,0.,1.20000004768372));
#5056=CARTESIAN_POINT('Origin',(60.4902124404907,0.,-1.59733337667944E-13));
#5057=CARTESIAN_POINT('',(60.4902111949971,0.,0.));
#5058=CARTESIAN_POINT('',(60.4902099491237,0.,27.2999995124759));
#5059=CARTESIAN_POINT('',(60.4902124404907,0.,0.));
#5060=CARTESIAN_POINT('Origin',(75.2228282332459,0.,4.9999999999998));
#5061=CARTESIAN_POINT('',(104.367515935362,-7.,5.00000000000001));
#5062=CARTESIAN_POINT('',(104.367515935362,0.,5.00000000000001));
#5063=CARTESIAN_POINT('',(75.2228282332459,-7.,4.9999999999998));
#5064=CARTESIAN_POINT('',(79.9288641879263,-7.,5.00000000000001));
#5065=CARTESIAN_POINT('',(75.2228282332459,0.,4.9999999999998));
#5066=CARTESIAN_POINT('',(75.2228282332459,0.,4.9999999999998));
#5067=CARTESIAN_POINT('',(9.99999999999999,0.,4.99999999999997));
#5068=CARTESIAN_POINT('Origin',(75.2228282332459,0.,7.99999999999986));
#5069=CARTESIAN_POINT('',(78.2228281586662,0.,8.00066893827696));
#5070=CARTESIAN_POINT('Origin',(75.2228282332459,0.,7.99999999999986));
#5071=CARTESIAN_POINT('',(78.2228281586662,-7.,8.00066893827696));
#5072=CARTESIAN_POINT('Origin',(75.2228282332459,-7.,7.99999999999986));
#5073=CARTESIAN_POINT('',(78.2228281586662,0.,8.00066893827696));
#5074=CARTESIAN_POINT('Origin',(78.2198407011243,0.,21.3985753059387));
#5075=CARTESIAN_POINT('',(78.2198405893095,0.,21.3985749218875));
#5076=CARTESIAN_POINT('',(78.2198407011243,0.,21.3985753059387));
#5077=CARTESIAN_POINT('',(78.2198405893095,-7.,21.3985749218875));
#5078=CARTESIAN_POINT('',(78.2198407011243,-7.,21.3985753059387));
#5079=CARTESIAN_POINT('',(78.2198407011243,0.,21.3985753059387));
#5080=CARTESIAN_POINT('Origin',(19.277690708776,0.,-53.4006744879114));
#5081=CARTESIAN_POINT('Origin',(19.277690708776,0.,-53.4006744879114));
#5082=CARTESIAN_POINT('Origin',(19.277690708776,-7.,-53.4006744879114));
#5083=CARTESIAN_POINT('Origin',(81.3189125061035,0.,25.3223204612732));
#5084=CARTESIAN_POINT('',(81.3189125061035,0.,25.3223204612732));
#5085=CARTESIAN_POINT('',(77.8756332397461,0.,27.9232501983643));
#5086=CARTESIAN_POINT('',(81.3189125061035,-7.,25.3223204612732));
#5087=CARTESIAN_POINT('',(77.8756332397461,-7.,27.9232501983643));
#5088=CARTESIAN_POINT('',(81.3189125061035,0.,25.3223204612732));
#5089=CARTESIAN_POINT('Origin',(78.2198407011243,0.,21.3985753059387));
#5090=CARTESIAN_POINT('',(83.2198429107666,0.,21.3985753059387));
#5091=CARTESIAN_POINT('Origin',(78.2198407011243,0.,21.3985753059387));
#5092=CARTESIAN_POINT('',(83.2198429107666,-7.,21.3985753059387));
#5093=CARTESIAN_POINT('Origin',(78.2198407011243,-7.,21.3985753059387));
#5094=CARTESIAN_POINT('',(83.2198429107666,0.,21.3985753059387));
#5095=CARTESIAN_POINT('Origin',(83.2198429107666,0.,14.7296345233917));
#5096=CARTESIAN_POINT('',(83.2198429107666,0.,14.7296345233917));
#5097=CARTESIAN_POINT('',(83.2198429107666,0.,14.7296345233917));
#5098=CARTESIAN_POINT('',(83.2198429107666,-7.,14.7296345233917));
#5099=CARTESIAN_POINT('',(83.2198429107666,-7.,14.7296345233917));
#5100=CARTESIAN_POINT('',(83.2198429107666,0.,14.7296345233917));
#5101=CARTESIAN_POINT('Origin',(87.219828801007,0.,14.7296358272062));
#5102=CARTESIAN_POINT('',(90.048246383667,0.,17.5580525398254));
#5103=CARTESIAN_POINT('Origin',(87.219828801007,0.,14.7296358272062));
#5104=CARTESIAN_POINT('',(90.048246383667,-7.,17.5580525398254));
#5105=CARTESIAN_POINT('Origin',(87.219828801007,-7.,14.7296358272062));
#5106=CARTESIAN_POINT('',(90.048246383667,0.,17.5580525398254));
#5107=CARTESIAN_POINT('Origin',(5.0000011920929,0.,0.));
#5108=CARTESIAN_POINT('',(102.131452560425,0.,0.));
#5109=CARTESIAN_POINT('',(0.,0.,0.));
#5110=CARTESIAN_POINT('',(102.131450259144,-7.,-1.35030875370034E-13));
#5111=CARTESIAN_POINT('',(102.131452560425,0.,0.));
#5112=CARTESIAN_POINT('',(102.131447957862,0.,-2.70061750740069E-13));
#5113=CARTESIAN_POINT('Origin',(102.131447957862,0.,2.99999999999972));
#5114=CARTESIAN_POINT('',(104.252768430411,0.,5.12132021457033));
#5115=CARTESIAN_POINT('Origin',(102.131447957862,0.,2.99999999999972));
#5116=CARTESIAN_POINT('',(104.252768430411,-7.,5.12132021457033));
#5117=CARTESIAN_POINT('',(104.252768430411,0.,5.12132021457033));
#5118=CARTESIAN_POINT('Origin',(102.131447957862,-7.,2.99999999999972));
#5119=CARTESIAN_POINT('Origin',(8.84896142591365,0.,103.000003814697));
#5120=CARTESIAN_POINT('',(6.72764075608762,0.,100.878683797404));
#5121=CARTESIAN_POINT('',(8.84896142591364,0.,106.000003814697));
#5122=CARTESIAN_POINT('Origin',(8.84896142591365,0.,103.000003814697));
#5123=CARTESIAN_POINT('',(6.72764075608761,-7.,100.878683797404));
#5124=CARTESIAN_POINT('',(6.72764075608762,0.,100.878683797404));
#5125=CARTESIAN_POINT('',(6.61290173218214,-7.,101.000003449436));
#5126=CARTESIAN_POINT('Origin',(8.84896142591365,-7.,103.000003814697));
#5127=CARTESIAN_POINT('',(8.84896917412274,-7.,106.000003814694));
#5128=CARTESIAN_POINT('Origin',(8.84896142591365,-7.,103.000003814697));
#5129=CARTESIAN_POINT('',(8.84896142591364,0.,106.000003814697));
#5130=CARTESIAN_POINT('Origin',(104.252768430411,0.,5.12132021457031));
#5131=CARTESIAN_POINT('',(20.9321784973145,0.,88.4419512748718));
#5132=CARTESIAN_POINT('',(20.9321784973145,0.,88.4419512748718));
#5133=CARTESIAN_POINT('',(20.9321784973145,-7.,88.4419512748718));
#5134=CARTESIAN_POINT('',(20.9321784973145,0.,88.4419512748718));
#5135=CARTESIAN_POINT('',(20.9321784973145,-7.,88.4419512748718));
#5136=CARTESIAN_POINT('Origin',(23.7605960799744,0.,91.2703679874911));
#5137=CARTESIAN_POINT('',(27.7605819702148,0.,91.2703692913056));
#5138=CARTESIAN_POINT('Origin',(23.7605960799744,0.,91.2703679874911));
#5139=CARTESIAN_POINT('',(27.7605819702148,-7.,91.2703692913056));
#5140=CARTESIAN_POINT('',(27.7605819702148,0.,91.2703692913056));
#5141=CARTESIAN_POINT('Origin',(23.7605960799744,-7.,91.2703679874911));
#5142=CARTESIAN_POINT('Origin',(27.7605819702148,0.,91.2703692913056));
#5143=CARTESIAN_POINT('',(27.7605819702148,0.,84.6014285087585));
#5144=CARTESIAN_POINT('',(27.7605819702148,0.,91.2703692913056));
#5145=CARTESIAN_POINT('',(27.7605819702148,-7.,84.6014285087585));
#5146=CARTESIAN_POINT('',(27.7605819702148,0.,84.6014285087585));
#5147=CARTESIAN_POINT('',(27.7605819702148,-7.,91.2703692913056));
#5148=CARTESIAN_POINT('Origin',(32.7605841798572,0.,84.6014285087586));
#5149=CARTESIAN_POINT('',(29.6615123748779,0.,80.6776833534241));
#5150=CARTESIAN_POINT('Origin',(32.7605841798572,0.,84.6014285087586));
#5151=CARTESIAN_POINT('',(29.6615123748779,-7.,80.6776833534241));
#5152=CARTESIAN_POINT('',(29.6615123748779,0.,80.6776833534241));
#5153=CARTESIAN_POINT('Origin',(32.7605841798572,-7.,84.6014285087586));
#5154=CARTESIAN_POINT('Origin',(32.7605841796355,0.,84.6014295030133));
#5155=CARTESIAN_POINT('',(32.7575967223152,0.,97.9993348764203));
#5156=CARTESIAN_POINT('',(32.7605841796355,0.,84.6014295030133));
#5157=CARTESIAN_POINT('',(32.7605841798572,0.,84.6014285087586));
#5158=CARTESIAN_POINT('',(32.7575967223152,-7.,97.9993348764203));
#5159=CARTESIAN_POINT('',(32.7575967223152,0.,97.9993348764203));
#5160=CARTESIAN_POINT('',(32.7605841796355,-7.,84.6014295030133));
#5161=CARTESIAN_POINT('',(32.7605841798572,-7.,84.6014285087586));
#5162=CARTESIAN_POINT('',(32.7605841796355,0.,84.6014295030133));
#5163=CARTESIAN_POINT('Origin',(35.7575966477356,0.,98.0000038146974));
#5164=CARTESIAN_POINT('',(35.7575966477355,0.,101.000003814697));
#5165=CARTESIAN_POINT('Origin',(35.7575966477356,0.,98.0000038146974));
#5166=CARTESIAN_POINT('',(35.7575966477355,-7.,101.000003814697));
#5167=CARTESIAN_POINT('',(35.7575966477355,0.,101.000003814697));
#5168=CARTESIAN_POINT('Origin',(35.7575966477356,-7.,98.0000038146974));
#5169=CARTESIAN_POINT('Origin',(8.84897692311915,0.,103.000003814698));
#5170=CARTESIAN_POINT('',(6.61290894561938,-8.,101.000003814698));
#5171=CARTESIAN_POINT('',(6.61290894561938,0.,101.000003814698));
#5172=CARTESIAN_POINT('',(8.84897692311919,-8.,106.000003814698));
#5173=CARTESIAN_POINT('Origin',(8.84897692311915,-8.,103.000003814698));
#5174=CARTESIAN_POINT('',(8.84897692311919,0.,106.000003814698));
#5175=CARTESIAN_POINT('Origin',(50.4902124404907,-8.,101.000003814697));
#5176=CARTESIAN_POINT('',(50.4902124404907,-8.,101.000003814697));
#5177=CARTESIAN_POINT('',(50.4902124404907,-8.,102.500009536743));
#5178=CARTESIAN_POINT('',(50.4902124404907,-8.,102.250003814697));
#5179=CARTESIAN_POINT('',(50.4902124404907,-2.,101.000003814697));
#5180=CARTESIAN_POINT('',(50.4902124404907,-4.,101.000003814697));
#5181=CARTESIAN_POINT('',(50.4902124404907,-2.,102.500009536743));
#5182=CARTESIAN_POINT('',(50.4902124404907,-2.,99.3318021496831));
#5183=CARTESIAN_POINT('',(50.4902124404907,-8.,102.500009536743));
#5184=CARTESIAN_POINT('Origin',(50.4902124404907,-8.,104.499998092651));
#5185=CARTESIAN_POINT('',(50.4902124404907,-8.,104.499998092651));
#5186=CARTESIAN_POINT('',(50.4902124404907,-8.,106.000003814697));
#5187=CARTESIAN_POINT('',(50.4902124404907,-8.,104.000000953674));
#5188=CARTESIAN_POINT('',(50.4902124404907,-2.,104.499998092651));
#5189=CARTESIAN_POINT('',(50.4902124404907,-8.,104.499998092651));
#5190=CARTESIAN_POINT('',(50.4902124404907,-2.,106.000003814697));
#5191=CARTESIAN_POINT('',(50.4902124404907,-2.,99.3318021496831));
#5192=CARTESIAN_POINT('',(50.4902124404907,-4.,106.000003814697));
#5193=CARTESIAN_POINT('Origin',(51.4902124404907,-9.00000013411045,105.000004768372));
#5194=CARTESIAN_POINT('',(51.4902124404907,-16.0000002384186,105.));
#5195=CARTESIAN_POINT('',(51.4902124404907,-16.0000002384186,105.708332061768));
#5196=CARTESIAN_POINT('',(51.4902124404907,-16.0000002384186,105.));
#5197=CARTESIAN_POINT('',(51.4902124404907,-2.00000000074881,106.000003814899));
#5198=CARTESIAN_POINT('',(51.4902124404907,-16.0000002384186,105.708332061768));
#5199=CARTESIAN_POINT('',(51.4902124404907,-2.00000000058142,105.));
#5200=CARTESIAN_POINT('',(51.4902124404907,-2.,105.125002861023));
#5201=CARTESIAN_POINT('',(51.4902124404907,-13.9999997615814,105.));
#5202=CARTESIAN_POINT('',(51.4902124404907,-13.9999997615814,105.));
#5203=CARTESIAN_POINT('',(51.4902124404907,-15.,104.000005722046));
#5204=CARTESIAN_POINT('',(51.4902124404907,-15.,104.000005722046));
#5205=CARTESIAN_POINT('',(51.4902124404907,-16.0000002384186,105.));
#5206=CARTESIAN_POINT('Origin',(51.4902124404907,-9.00000013411045,102.000002861023));
#5207=CARTESIAN_POINT('',(51.4902124404907,-16.0000002384186,101.291675567627));
#5208=CARTESIAN_POINT('',(51.4902124404907,-16.0000002384186,102.000007629395));
#5209=CARTESIAN_POINT('',(51.4902124404907,-16.0000002384186,101.291675567627));
#5210=CARTESIAN_POINT('',(51.4902124404907,-15.,103.000001907349));
#5211=CARTESIAN_POINT('',(51.4902124404907,-16.0000002384186,102.000007629395));
#5212=CARTESIAN_POINT('',(51.4902124404907,-13.9999997615814,102.000007629395));
#5213=CARTESIAN_POINT('',(51.4902124404907,-15.,103.000001907349));
#5214=CARTESIAN_POINT('',(51.4902124404907,-2.00000000058142,102.000007629395));
#5215=CARTESIAN_POINT('',(51.4902124404907,-13.9999997615814,102.000007629395));
#5216=CARTESIAN_POINT('',(51.4902124404907,-2.00000000074881,101.000003814495));
#5217=CARTESIAN_POINT('',(51.4902124404907,-2.,101.875004768372));
#5218=CARTESIAN_POINT('',(51.4902124404907,-16.0000002384186,101.291675567627));
#5219=CARTESIAN_POINT('Origin',(6.72764075608762,0.,100.878683797404));
#5220=CARTESIAN_POINT('',(6.72764075608762,-7.,100.878683797404));
#5221=CARTESIAN_POINT('',(6.72764075608762,0.,100.878683797404));
#5222=CARTESIAN_POINT('Origin',(91.7027341722054,0.,159.400678302609));
#5223=CARTESIAN_POINT('',(110.980424880981,0.,61.0401487350464));
#5224=CARTESIAN_POINT('Origin',(91.7027341722054,0.,159.400678302609));
#5225=CARTESIAN_POINT('',(110.980424880981,-7.,61.0401487350464));
#5226=CARTESIAN_POINT('',(110.980424880981,0.,61.0401487350464));
#5227=CARTESIAN_POINT('Origin',(91.7027341722054,-7.,159.400678302609));
#5228=CARTESIAN_POINT('Origin',(110.980424880981,0.,61.0401487350464));
#5229=CARTESIAN_POINT('',(110.980424880981,0.,101.000003814697));
#5230=CARTESIAN_POINT('',(110.980424880981,0.,101.000003814697));
#5231=CARTESIAN_POINT('',(110.980424880981,-7.,101.000003814697));
#5232=CARTESIAN_POINT('',(110.980424880981,0.,101.000003814697));
#5233=CARTESIAN_POINT('',(110.980424880981,-7.,101.000003814697));
#5234=CARTESIAN_POINT('Origin',(105.980424880981,0.,101.000003814697));
#5235=CARTESIAN_POINT('',(105.980424880981,0.,106.000003814697));
#5236=CARTESIAN_POINT('Origin',(105.980424880981,0.,101.000003814697));
#5237=CARTESIAN_POINT('',(105.980424880981,-8.,106.000003814697));
#5238=CARTESIAN_POINT('',(105.980424880981,0.,106.000003814697));
#5239=CARTESIAN_POINT('',(110.980424880981,-8.,101.000003814697));
#5240=CARTESIAN_POINT('Origin',(105.980424880981,-8.,101.000003814697));
#5241=CARTESIAN_POINT('',(110.980424880981,0.,101.000003814697));
#5242=CARTESIAN_POINT('Origin',(105.980424880981,0.,106.000003814697));
#5243=CARTESIAN_POINT('',(59.4902124404907,-2.00000000074881,106.000003814899));
#5244=CARTESIAN_POINT('',(80.7353186607361,-2.,106.000003814697));
#5245=CARTESIAN_POINT('',(60.4902124404907,-2.,106.000003814697));
#5246=CARTESIAN_POINT('',(80.7353186607361,-2.,106.000003814697));
#5247=CARTESIAN_POINT('',(60.4902124404907,-8.,106.000003814697));
#5248=CARTESIAN_POINT('',(60.4902124404907,-4.,106.000003814697));
#5249=CARTESIAN_POINT('',(105.980424880981,-8.,106.000003814697));
#5250=CARTESIAN_POINT('',(110.980424880981,0.,106.000003814697));
#5251=CARTESIAN_POINT('',(105.980424880981,-8.,106.000003814697));
#5252=CARTESIAN_POINT('',(80.7353186607361,-2.,106.000003814697));
#5253=CARTESIAN_POINT('Origin',(100.980424880981,0.,96.0000038146973));
#5254=CARTESIAN_POINT('',(105.980424880981,0.,96.0000038146973));
#5255=CARTESIAN_POINT('',(100.980424880981,0.,101.000003814697));
#5256=CARTESIAN_POINT('Origin',(100.980424880981,0.,96.0000038146973));
#5257=CARTESIAN_POINT('',(105.980424880981,-7.,96.0000038146973));
#5258=CARTESIAN_POINT('',(105.980424880981,0.,96.0000038146973));
#5259=CARTESIAN_POINT('',(100.980424880981,-7.,101.000003814697));
#5260=CARTESIAN_POINT('Origin',(100.980424880981,-7.,96.0000038146973));
#5261=CARTESIAN_POINT('',(100.980424880981,0.,101.000003814697));
#5262=CARTESIAN_POINT('Origin',(105.980424880981,0.,96.0000038146973));
#5263=CARTESIAN_POINT('',(105.980424880981,0.,65.2452099815658));
#5264=CARTESIAN_POINT('',(105.980424880981,0.,96.0000038146973));
#5265=CARTESIAN_POINT('',(105.980424880981,-7.,65.2452099815658));
#5266=CARTESIAN_POINT('',(105.980424880981,0.,65.2452099815658));
#5267=CARTESIAN_POINT('',(105.980424880981,-7.,96.0000038146973));
#5268=CARTESIAN_POINT('Origin',(55.4902124404907,-7.,53.0000019073488));
#5269=CARTESIAN_POINT('',(31.0515606930551,-7.,101.000003814697));
#5270=CARTESIAN_POINT('Origin',(91.7027341722054,-7.,159.400678302609));
#5271=CARTESIAN_POINT('',(31.0515606930551,-7.,101.000003814697));
#5272=CARTESIAN_POINT('Origin',(100.979998908817,0.,103.499990047768));
#5273=CARTESIAN_POINT('',(99.2299966192206,-2.8,103.499990047768));
#5274=CARTESIAN_POINT('Origin',(100.979998908817,-2.8,103.499990047768));
#5275=CARTESIAN_POINT('',(99.2299966192206,-8.,103.499990047768));
#5276=CARTESIAN_POINT('',(99.2299966192206,0.,103.499990047768));
#5277=CARTESIAN_POINT('Origin',(100.979998908817,-8.,103.499990047768));
#5278=CARTESIAN_POINT('Origin',(100.979998908817,-2.8,103.499990047768));
#5279=CARTESIAN_POINT('Origin',(60.4902124404907,-8.,102.500009536743));
#5280=CARTESIAN_POINT('',(60.4902124404907,-8.,102.500009536743));
#5281=CARTESIAN_POINT('',(60.4902124404907,-8.,101.000003814697));
#5282=CARTESIAN_POINT('',(60.4902124404907,-8.,103.00000667572));
#5283=CARTESIAN_POINT('',(60.4902124404907,-2.,102.500009536743));
#5284=CARTESIAN_POINT('',(60.4902124404907,-8.,102.500009536743));
#5285=CARTESIAN_POINT('',(60.4902124404907,-2.,101.000003814697));
#5286=CARTESIAN_POINT('',(60.4902124404907,-2.,107.453377863095));
#5287=CARTESIAN_POINT('',(60.4902124404907,-4.,101.000003814697));
#5288=CARTESIAN_POINT('Origin',(55.4902124404907,-2.,105.250000953674));
#5289=CARTESIAN_POINT('',(60.4902124404907,-2.,104.499998092651));
#5290=CARTESIAN_POINT('',(50.4902124404907,-2.,104.499998092651));
#5291=CARTESIAN_POINT('',(60.4902124404907,-2.,107.453377863095));
#5292=CARTESIAN_POINT('',(59.4902124404907,-2.00000000058142,105.));
#5293=CARTESIAN_POINT('',(59.4902124404907,-2.,105.125002861023));
#5294=CARTESIAN_POINT('',(55.4902124404907,-2.,105.));
#5295=CARTESIAN_POINT('Origin',(60.4902124404907,-8.,106.000003814697));
#5296=CARTESIAN_POINT('',(60.4902124404907,-8.,104.499998092651));
#5297=CARTESIAN_POINT('',(60.4902124404907,-8.,104.750003814697));
#5298=CARTESIAN_POINT('',(60.4902124404907,-8.,104.499998092651));
#5299=CARTESIAN_POINT('Origin',(60.4902124404907,-8.,104.499998092651));
#5300=CARTESIAN_POINT('',(59.4524566712705,-8.,104.499998092651));
#5301=CARTESIAN_POINT('Origin',(55.4902124404907,-16.0000002384186,105.));
#5302=CARTESIAN_POINT('',(59.4902124404907,-16.0000002384186,105.));
#5303=CARTESIAN_POINT('',(55.4902124404907,-16.0000002384186,105.));
#5304=CARTESIAN_POINT('',(59.4902124404907,-16.0000002384186,105.708332061768));
#5305=CARTESIAN_POINT('',(59.4902124404907,-16.0000002384186,105.));
#5306=CARTESIAN_POINT('',(55.4902124404907,-16.0000002384186,105.708332061768));
#5307=CARTESIAN_POINT('Origin',(55.4902124404907,-16.0000002384186,105.708332061768));
#5308=CARTESIAN_POINT('',(59.4902124404907,-16.0000002384186,105.708332061768));
#5309=CARTESIAN_POINT('Origin',(55.4902124404907,-2.00000002980232,105.));
#5310=CARTESIAN_POINT('',(59.4902124404907,-13.9999997615814,105.));
#5311=CARTESIAN_POINT('',(59.4902124404907,-13.9999997615814,105.));
#5312=CARTESIAN_POINT('',(55.4902124404907,-13.9999997615814,105.));
#5313=CARTESIAN_POINT('Origin',(55.4902124404907,-13.9999997615814,105.));
#5314=CARTESIAN_POINT('',(59.4902124404907,-15.,104.000005722046));
#5315=CARTESIAN_POINT('',(59.4902124404907,-15.,104.000005722046));
#5316=CARTESIAN_POINT('',(55.4902124404907,-15.,104.000005722046));
#5317=CARTESIAN_POINT('Origin',(55.4902124404907,-15.,104.000005722046));
#5318=CARTESIAN_POINT('',(59.4902124404907,-16.0000002384186,105.));
#5319=CARTESIAN_POINT('Origin',(59.4902124404907,-9.00000013411045,105.000004768372));
#5320=CARTESIAN_POINT('Origin',(59.4902124404907,-9.00000013411045,102.000002861023));
#5321=CARTESIAN_POINT('',(59.4902124404907,-16.0000002384186,102.000007629395));
#5322=CARTESIAN_POINT('',(59.4902124404907,-16.0000002384186,101.291675567627));
#5323=CARTESIAN_POINT('',(59.4902124404907,-16.0000002384186,101.291675567627));
#5324=CARTESIAN_POINT('',(59.4902124404907,-2.00000000074881,101.000003814495));
#5325=CARTESIAN_POINT('',(59.4902124404907,-16.0000002384186,101.291675567627));
#5326=CARTESIAN_POINT('',(59.4902124404907,-2.00000000058142,102.000007629395));
#5327=CARTESIAN_POINT('',(59.4902124404907,-2.,101.875004768372));
#5328=CARTESIAN_POINT('',(59.4902124404907,-13.9999997615814,102.000007629395));
#5329=CARTESIAN_POINT('',(59.4902124404907,-13.9999997615814,102.000007629395));
#5330=CARTESIAN_POINT('',(59.4902124404907,-15.,103.000001907349));
#5331=CARTESIAN_POINT('',(59.4902124404907,-15.,103.000001907349));
#5332=CARTESIAN_POINT('',(59.4902124404907,-16.0000002384186,102.000007629395));
#5333=CARTESIAN_POINT('Origin',(55.4902124404907,0.,53.0000019073488));
#5334=CARTESIAN_POINT('Origin',(91.7027341722054,0.,159.400678302609));
#5335=CARTESIAN_POINT('',(100.980424880981,0.,101.000003814697));
#5336=CARTESIAN_POINT('Origin',(91.7027341722054,0.,159.400678302609));
#5337=CARTESIAN_POINT('Origin',(35.7575966477355,0.,101.000003814697));
#5338=CARTESIAN_POINT('',(118.228700328537,-8.,101.000003814697));
#5339=CARTESIAN_POINT('',(45.6239045441131,-2.,101.000003814697));
#5340=CARTESIAN_POINT('',(45.6239045441131,-2.,101.000003814697));
#5341=CARTESIAN_POINT('',(45.6239045441131,-2.,101.000003814697));
#5342=CARTESIAN_POINT('',(118.228700328537,-8.,101.000003814697));
#5343=CARTESIAN_POINT('Origin',(55.4902124404907,-2.00000002980232,101.000003814697));
#5344=CARTESIAN_POINT('',(55.4902124404907,-16.0000002384186,101.291675567627));
#5345=CARTESIAN_POINT('Origin',(55.4902124404907,-16.0000002384186,101.291675567627));
#5346=CARTESIAN_POINT('',(55.4902124404907,-16.0000002384186,102.000007629395));
#5347=CARTESIAN_POINT('Origin',(55.4902124404907,-16.0000002384186,102.000007629395));
#5348=CARTESIAN_POINT('',(55.4902124404907,-15.,103.000001907349));
#5349=CARTESIAN_POINT('Origin',(55.4902124404907,-15.,103.000001907349));
#5350=CARTESIAN_POINT('',(55.4902124404907,-13.9999997615814,102.000007629395));
#5351=CARTESIAN_POINT('Origin',(55.4902124404907,-13.9999997615814,102.000007629395));
#5352=CARTESIAN_POINT('',(55.4902124404907,-2.,102.000007629395));
#5353=CARTESIAN_POINT('Origin',(55.4902124404907,-2.,101.75000667572));
#5354=CARTESIAN_POINT('',(50.4902124404907,-2.,102.500009536743));
#5355=CARTESIAN_POINT('Origin',(50.4902124404907,-8.,102.500009536743));
#5356=CARTESIAN_POINT('',(54.4524566712705,-8.,102.500009536743));
#5357=CARTESIAN_POINT('Origin',(58.4147009020503,-8.,103.500003814697));
#5358=CARTESIAN_POINT('',(0.,0.,0.));
#5359=CARTESIAN_POINT('Origin',(55.4902124404907,-4.00000013411045,0.145828066207017));
#5360=CARTESIAN_POINT('',(54.1678121566157,-5.5000937214608,0.177080560468535));
#5361=CARTESIAN_POINT('',(56.8126127243658,-5.5000937214608,0.177080560468536));
#5362=CARTESIAN_POINT('',(55.4902111948072,-5.5000937214608,0.177080560468535));
#5363=CARTESIAN_POINT('Origin',(55.4902124404907,-4.00000013411045,0.145828066207017));
#5364=CARTESIAN_POINT('Origin',(55.4902124404907,-4.00000013411045,0.145828066207017));
#5365=CARTESIAN_POINT('',(55.7596018087023,-2.00000023841859,0.999999909568344));
#5366=CARTESIAN_POINT('',(53.4902124404907,-3.98220457731446,0.999999909568344));
#5367=CARTESIAN_POINT('Origin',(55.4902124404907,-3.98220457731446,0.999999909568344));
#5368=CARTESIAN_POINT('',(55.2208230722792,-2.00000023841859,0.999999909568344));
#5369=CARTESIAN_POINT('Origin',(55.4902124404907,-4.02437963145607,-1.02436741723056));
#5370=CARTESIAN_POINT('Origin',(55.4902124404907,-3.98220457731446,0.999999909568344));
#5371=CARTESIAN_POINT('',(53.4902124404907,-3.99869735870019,0.208360196357335));
#5372=CARTESIAN_POINT('',(53.4902124404907,-4.00000013411045,0.145828066207016));
#5373=CARTESIAN_POINT('Origin',(55.4902124404907,-3.9986973587002,0.208360196357335));
#5374=CARTESIAN_POINT('Origin',(55.4902124404907,-3.9986973587002,0.208360196357335));
#5375=CARTESIAN_POINT('Origin',(55.4902124404907,-4.00000013411045,0.145828066207017));
#5376=CARTESIAN_POINT('',(53.4902124404907,-3.90325229314834,4.78964351987318));
#5377=CARTESIAN_POINT('Origin',(55.4902124404907,-3.90325229314834,4.78964351987318));
#5378=CARTESIAN_POINT('',(53.4902124404907,-3.91970364728078,3.99999228017381));
#5379=CARTESIAN_POINT('',(53.4902124404907,-4.00000013411045,0.145828066207016));
#5380=CARTESIAN_POINT('',(54.9277733864728,-2.00000023841859,3.99999228017381));
#5381=CARTESIAN_POINT('Origin',(55.4902124404907,-3.91970364728078,3.99999228017381));
#5382=CARTESIAN_POINT('',(56.0526514945086,-2.00000023841859,3.99999228017381));
#5383=CARTESIAN_POINT('Origin',(55.4902124404907,-3.88052558675829,5.88050641971165));
#5384=CARTESIAN_POINT('Origin',(55.4902124404907,-3.91970364728078,3.99999228017381));
#5385=CARTESIAN_POINT('Origin',(55.4902099491237,-2.00000023841859,3.99999228017381));
#5386=CARTESIAN_POINT('',(59.4902099491237,-2.00000023841859,3.99999228017381));
#5387=CARTESIAN_POINT('',(55.4902099491237,-2.00000023841859,3.99999228017381));
#5388=CARTESIAN_POINT('',(59.4902099491237,-13.9999999994186,3.99999228017381));
#5389=CARTESIAN_POINT('',(59.4902099491237,-2.00000023841859,3.99999228017381));
#5390=CARTESIAN_POINT('',(51.4902099491237,-13.9999999994186,3.99999228017381));
#5391=CARTESIAN_POINT('',(55.4902099491237,-14.,3.99999228017381));
#5392=CARTESIAN_POINT('',(51.4902099491237,-2.00000023841859,3.99999228017381));
#5393=CARTESIAN_POINT('',(51.4902099491237,-2.00000023841859,3.99999228017381));
#5394=CARTESIAN_POINT('',(55.4902099491237,-2.00000023841859,3.99999228017381));
#5395=CARTESIAN_POINT('Origin',(55.4902099491237,-13.9999999701977,0.999999909568344));
#5396=CARTESIAN_POINT('',(51.4902099491237,-2.00000023841859,0.999999909568344));
#5397=CARTESIAN_POINT('',(55.4902099491237,-2.00000023841859,0.999999909568344));
#5398=CARTESIAN_POINT('',(51.4902099491237,-13.9999999994186,0.999999909568344));
#5399=CARTESIAN_POINT('',(51.4902099491237,-2.00000023841859,0.999999909568344));
#5400=CARTESIAN_POINT('',(59.4902099491237,-13.9999999994186,0.999999909568344));
#5401=CARTESIAN_POINT('',(55.4902099491237,-14.,0.999999909568344));
#5402=CARTESIAN_POINT('',(59.4902099491237,-2.00000023841859,0.999999909568344));
#5403=CARTESIAN_POINT('',(59.4902099491237,-2.00000023841859,0.999999909568344));
#5404=CARTESIAN_POINT('',(55.4902099491237,-2.00000023841859,0.999999909568344));
#5405=CARTESIAN_POINT('Origin',(55.4902124404907,-12.0000001341105,105.854167938232));
#5406=CARTESIAN_POINT('',(53.4902124404907,-11.9780379165298,104.799999861885));
#5407=CARTESIAN_POINT('Origin',(55.4902124404907,-11.9780379165298,104.799999861885));
#5408=CARTESIAN_POINT('',(53.4902124404907,-11.9213427352736,102.078678577114));
#5409=CARTESIAN_POINT('',(53.4902124404907,-12.0000001341105,105.854167938232));
#5410=CARTESIAN_POINT('Origin',(55.4902124404907,-11.9213427352736,102.078678577114));
#5411=CARTESIAN_POINT('Origin',(10.0000020566038,-4.00000000000001,2.50000086324266));
#5412=CARTESIAN_POINT('',(11.500002191775,-8.,2.50000086324266));
#5413=CARTESIAN_POINT('Origin',(10.0000020566037,-8.,2.50000086324266));
#5414=CARTESIAN_POINT('',(11.500002191775,-12.,2.50000086324266));
#5415=CARTESIAN_POINT('',(11.500002191775,-4.00000000000001,2.50000086324266));
#5416=CARTESIAN_POINT('Origin',(10.0000020566038,-12.,2.50000086324266));
#5417=CARTESIAN_POINT('Origin',(10.0000020566038,-12.,2.50000086324266));
#5418=CARTESIAN_POINT('Origin',(100.979994297411,-4.00000000000001,103.500004749034));
#5419=CARTESIAN_POINT('',(102.479993922177,-8.00000000000001,103.500004749034));
#5420=CARTESIAN_POINT('Origin',(100.979994297411,-8.00000000000001,103.500004749034));
#5421=CARTESIAN_POINT('',(102.479993922177,-12.,103.500004749034));
#5422=CARTESIAN_POINT('',(102.479993922178,-4.00000000000001,103.500004749034));
#5423=CARTESIAN_POINT('Origin',(100.979994297411,-12.,103.500004749034));
#5424=CARTESIAN_POINT('Origin',(100.979994297411,-12.,103.500004749034));
#5425=CARTESIAN_POINT('Origin',(110.980422389614,-16.,44.959851174522));
#5426=CARTESIAN_POINT('',(110.980422389614,-16.,4.9999960948711));
#5427=CARTESIAN_POINT('',(110.980422389614,-16.,44.959851174522));
#5428=CARTESIAN_POINT('',(110.980422389614,-16.,4.9999960948711));
#5429=CARTESIAN_POINT('',(110.980422389614,-9.00000000000001,4.9999960948711));
#5430=CARTESIAN_POINT('',(110.980422389614,-16.,4.9999960948711));
#5431=CARTESIAN_POINT('',(110.980422389614,-9.00000000000001,44.959851174522));
#5432=CARTESIAN_POINT('',(110.980422389614,-9.00000000000001,4.9999960948711));
#5433=CARTESIAN_POINT('',(110.980422389614,-16.,44.959851174522));
#5434=CARTESIAN_POINT('Origin',(105.980422389614,-16.,4.99999609487108));
#5435=CARTESIAN_POINT('',(105.980422389614,-16.,-3.90512892134431E-6));
#5436=CARTESIAN_POINT('Origin',(105.980422389614,-16.,4.99999609487108));
#5437=CARTESIAN_POINT('',(105.980422389614,-8.00000000000001,-3.90512892134431E-6));
#5438=CARTESIAN_POINT('',(105.980422389614,-16.,-3.90512892134431E-6));
#5439=CARTESIAN_POINT('',(110.980422389614,-8.00000000000001,4.99999609487108));
#5440=CARTESIAN_POINT('Origin',(105.980422389614,-8.00000000000001,4.99999609487108));
#5441=CARTESIAN_POINT('',(110.980422389614,-16.,4.99999609487108));
#5442=CARTESIAN_POINT('Origin',(100.980422389614,-16.,9.99999609487106));
#5443=CARTESIAN_POINT('',(105.980422389614,-16.,9.99999609487106));
#5444=CARTESIAN_POINT('',(100.980422389614,-16.,4.99999609487106));
#5445=CARTESIAN_POINT('Origin',(100.980422389614,-16.,9.99999609487106));
#5446=CARTESIAN_POINT('',(105.980422389614,-9.00000000000001,9.99999609487106));
#5447=CARTESIAN_POINT('',(105.980422389614,-16.,9.99999609487106));
#5448=CARTESIAN_POINT('',(100.980422389614,-9.00000000000001,4.99999609487106));
#5449=CARTESIAN_POINT('Origin',(100.980422389614,-9.00000000000001,9.99999609487106));
#5450=CARTESIAN_POINT('',(100.980422389614,-16.,4.99999609487106));
#5451=CARTESIAN_POINT('Origin',(105.980422389614,-16.,9.99999609487106));
#5452=CARTESIAN_POINT('',(105.980422389614,-16.,40.7547899280026));
#5453=CARTESIAN_POINT('',(105.980422389614,-16.,9.99999609487106));
#5454=CARTESIAN_POINT('',(105.980422389614,-9.00000000000001,40.7547899280026));
#5455=CARTESIAN_POINT('',(105.980422389614,-16.,40.7547899280026));
#5456=CARTESIAN_POINT('',(105.980422389614,-9.00000000000001,9.99999609487106));
#5457=CARTESIAN_POINT('Origin',(100.97999641745,-16.,2.50000986180084));
#5458=CARTESIAN_POINT('',(99.2299941278536,-13.2,2.50000986180084));
#5459=CARTESIAN_POINT('Origin',(100.97999641745,-13.2,2.50000986180084));
#5460=CARTESIAN_POINT('',(99.2299941278536,-8.00000000000001,2.50000986180084));
#5461=CARTESIAN_POINT('',(99.2299941278536,-16.,2.50000986180084));
#5462=CARTESIAN_POINT('Origin',(100.97999641745,-8.00000000000001,2.50000986180084));
#5463=CARTESIAN_POINT('Origin',(100.97999641745,-13.2,2.50000986180084));
#5464=CARTESIAN_POINT('Origin',(60.4902099491237,-8.00000000000001,3.49999037282518));
#5465=CARTESIAN_POINT('',(60.4902099491237,-8.00000000000001,3.49999037282518));
#5466=CARTESIAN_POINT('',(60.4902099491237,-8.00000000000001,4.99999609487094));
#5467=CARTESIAN_POINT('',(60.4902099491237,-8.00000000000001,2.99999323384806));
#5468=CARTESIAN_POINT('',(60.4902099491237,-14.,3.49999037282518));
#5469=CARTESIAN_POINT('',(60.4902099491237,-8.00000000000001,3.49999037282518));
#5470=CARTESIAN_POINT('',(60.4902099491237,-14.,4.99999609487094));
#5471=CARTESIAN_POINT('',(60.4902099491237,-14.,-1.45337795352698));
#5472=CARTESIAN_POINT('',(60.4902099491237,-12.,4.99999609487094));
#5473=CARTESIAN_POINT('Origin',(60.4902099491237,-8.00000000000001,-3.90512906345286E-6));
#5474=CARTESIAN_POINT('',(60.4902099491237,-8.00000000000001,-3.90512906345286E-6));
#5475=CARTESIAN_POINT('',(60.4902099491237,-8.00000000000001,1.50000181691698));
#5476=CARTESIAN_POINT('',(60.4902099491237,-8.00000000000001,1.24999609487094));
#5477=CARTESIAN_POINT('',(60.4902099491237,-14.,-3.90512906345286E-6));
#5478=CARTESIAN_POINT('',(60.4902099491237,-12.,-3.90512892134431E-6));
#5479=CARTESIAN_POINT('',(60.4902099491237,-14.,1.50000181691698));
#5480=CARTESIAN_POINT('',(60.4902099491237,-14.,-1.45337795352698));
#5481=CARTESIAN_POINT('',(60.4902099491237,-8.00000000000001,1.50000181691698));
#5482=CARTESIAN_POINT('Origin',(59.4902099491237,-6.99999986588956,0.999995141196762));
#5483=CARTESIAN_POINT('',(59.4902099491237,2.38418571552046E-7,0.291667847800766));
#5484=CARTESIAN_POINT('',(59.4902099491237,2.38418571552046E-7,0.999999909568344));
#5485=CARTESIAN_POINT('',(59.4902099491237,2.38418571552046E-7,0.999999909568344));
#5486=CARTESIAN_POINT('',(59.4902099491237,-1.00000000000001,1.99999418752245));
#5487=CARTESIAN_POINT('',(59.4902099491237,2.38418571552046E-7,0.999999909568344));
#5488=CARTESIAN_POINT('',(59.4902099491237,-1.00000000000001,1.99999418752245));
#5489=CARTESIAN_POINT('',(59.4902099491237,-13.9999999992512,-3.90533088293397E-6));
#5490=CARTESIAN_POINT('',(59.4902099491237,-14.,0.87499704854536));
#5491=CARTESIAN_POINT('',(59.4902099491237,2.38418571552046E-7,0.291667847800766));
#5492=CARTESIAN_POINT('Origin',(59.4902099491237,-6.99999986588956,3.99999704854539));
#5493=CARTESIAN_POINT('',(59.4902099491237,2.38418571552046E-7,3.99999228017381));
#5494=CARTESIAN_POINT('',(59.4902099491237,2.38418571552046E-7,4.70832434194139));
#5495=CARTESIAN_POINT('',(59.4902099491237,2.38418571552046E-7,4.70832434194139));
#5496=CARTESIAN_POINT('',(59.4902099491237,-13.9999999992512,4.99999609507296));
#5497=CARTESIAN_POINT('',(59.4902099491237,2.38418571552046E-7,4.70832434194139));
#5498=CARTESIAN_POINT('',(59.4902099491237,-14.,4.12499514119673));
#5499=CARTESIAN_POINT('',(59.4902099491237,-1.00000000000001,2.99999800221971));
#5500=CARTESIAN_POINT('',(59.4902099491237,-1.00000000000001,2.99999800221971));
#5501=CARTESIAN_POINT('',(59.4902099491237,2.38418571552046E-7,3.99999228017381));
#5502=CARTESIAN_POINT('Origin',(8.84895893454662,-16.,2.99999609487109));
#5503=CARTESIAN_POINT('',(6.72763826472058,-16.,5.1213161121643));
#5504=CARTESIAN_POINT('',(8.84895893454661,-16.,-3.90512892134431E-6));
#5505=CARTESIAN_POINT('Origin',(8.84895893454662,-16.,2.99999609487109));
#5506=CARTESIAN_POINT('',(6.72763826472058,-9.,5.1213161121643));
#5507=CARTESIAN_POINT('',(6.72763826472058,-16.,5.1213161121643));
#5508=CARTESIAN_POINT('',(6.61289924081467,-9.,4.99999646013235));
#5509=CARTESIAN_POINT('Origin',(8.84895893454662,-9.,2.99999609487109));
#5510=CARTESIAN_POINT('',(8.84896668275571,-9.,-3.90512567523723E-6));
#5511=CARTESIAN_POINT('Origin',(8.84895893454662,-9.,2.99999609487109));
#5512=CARTESIAN_POINT('',(8.84895893454661,-16.,-3.90512892134431E-6));
#5513=CARTESIAN_POINT('Origin',(23.7605935886074,-16.,14.7296319220772));
#5514=CARTESIAN_POINT('',(20.9321760059474,-16.,17.5580486346965));
#5515=CARTESIAN_POINT('',(27.7605794788478,-16.,14.7296306182628));
#5516=CARTESIAN_POINT('Origin',(23.7605935886074,-16.,14.7296319220772));
#5517=CARTESIAN_POINT('',(27.7605794788478,-9.,14.7296306182628));
#5518=CARTESIAN_POINT('',(27.7605794788478,-16.,14.7296306182628));
#5519=CARTESIAN_POINT('',(20.9321760059474,-9.,17.5580486346965));
#5520=CARTESIAN_POINT('Origin',(23.7605935886074,-9.,14.7296319220772));
#5521=CARTESIAN_POINT('',(20.9321760059474,-16.,17.5580486346965));
#5522=CARTESIAN_POINT('Origin',(27.7605794788478,-16.,14.7296306182628));
#5523=CARTESIAN_POINT('',(27.7605794788478,-16.,21.3985714008098));
#5524=CARTESIAN_POINT('',(27.7605794788478,-16.,14.7296306182628));
#5525=CARTESIAN_POINT('',(27.7605794788478,-9.,21.3985714008098));
#5526=CARTESIAN_POINT('',(27.7605794788478,-16.,21.3985714008098));
#5527=CARTESIAN_POINT('',(27.7605794788478,-9.,14.7296306182628));
#5528=CARTESIAN_POINT('Origin',(32.7605816884901,-16.,21.3985714008098));
#5529=CARTESIAN_POINT('',(29.6615098835109,-16.,25.3223165561443));
#5530=CARTESIAN_POINT('Origin',(32.7605816884901,-16.,21.3985714008098));
#5531=CARTESIAN_POINT('',(29.6615098835109,-9.,25.3223165561443));
#5532=CARTESIAN_POINT('',(29.6615098835109,-16.,25.3223165561443));
#5533=CARTESIAN_POINT('Origin',(32.7605816884901,-9.00000000000001,21.3985714008098));
#5534=CARTESIAN_POINT('Origin',(91.7027316808384,-16.,-53.4006783930403));
#5535=CARTESIAN_POINT('',(32.7605816882684,-16.,21.3985704065551));
#5536=CARTESIAN_POINT('Origin',(91.7027316808384,-16.,-53.4006783930403));
#5537=CARTESIAN_POINT('',(32.7605816882684,-9.00000000000001,21.3985704065551));
#5538=CARTESIAN_POINT('',(32.7605816882684,-16.,21.3985704065551));
#5539=CARTESIAN_POINT('Origin',(91.7027316808384,-9.00000000000001,-53.4006783930403));
#5540=CARTESIAN_POINT('Origin',(32.7605816882684,-16.,21.3985704065551));
#5541=CARTESIAN_POINT('',(32.7575942309482,-16.,8.00066503314802));
#5542=CARTESIAN_POINT('',(32.7605816884901,-16.,21.3985714008098));
#5543=CARTESIAN_POINT('',(32.7575942309482,-9.00000000000001,8.00066503314802));
#5544=CARTESIAN_POINT('',(32.7575942309482,-16.,8.00066503314802));
#5545=CARTESIAN_POINT('',(32.7605816884901,-9.00000000000001,21.3985714008098));
#5546=CARTESIAN_POINT('Origin',(35.7575941563685,-16.,7.99999609487094));
#5547=CARTESIAN_POINT('',(35.7575941563685,-16.,4.99999609487087));
#5548=CARTESIAN_POINT('Origin',(35.7575941563685,-16.,7.99999609487094));
#5549=CARTESIAN_POINT('',(35.7575941563685,-9.00000000000001,4.99999609487087));
#5550=CARTESIAN_POINT('',(35.7575941563685,-16.,4.99999609487087));
#5551=CARTESIAN_POINT('Origin',(35.7575941563685,-9.00000000000001,7.99999609487094));
#5552=CARTESIAN_POINT('Origin',(35.7575941563685,-16.,4.99999609487087));
#5553=CARTESIAN_POINT('',(51.4902099491237,-13.9999999992512,4.99999609507295));
#5554=CARTESIAN_POINT('',(45.6239020527461,-14.,4.9999960948709));
#5555=CARTESIAN_POINT('',(50.4902099491237,-14.,4.9999960948709));
#5556=CARTESIAN_POINT('',(45.6239020527461,-14.,4.9999960948709));
#5557=CARTESIAN_POINT('',(50.4902099491237,-8.00000000000001,4.9999960948709));
#5558=CARTESIAN_POINT('',(50.4902099491237,-12.,4.9999960948709));
#5559=CARTESIAN_POINT('',(6.61290645425235,-8.,4.99999609487078));
#5560=CARTESIAN_POINT('',(118.22869783717,-8.00000000000002,4.9999960948711));
#5561=CARTESIAN_POINT('',(6.61290645425235,-16.,4.99999609487078));
#5562=CARTESIAN_POINT('',(31.0515582016881,-9.,4.99999609487085));
#5563=CARTESIAN_POINT('',(100.980422389614,-16.,4.99999609487106));
#5564=CARTESIAN_POINT('',(31.0515582016881,-9.,4.99999609487085));
#5565=CARTESIAN_POINT('',(118.22869783717,-8.00000000000002,4.9999960948711));
#5566=CARTESIAN_POINT('',(45.6239020527461,-14.,4.9999960948709));
#5567=CARTESIAN_POINT('Origin',(8.84897443175212,-16.,2.99999609487078));
#5568=CARTESIAN_POINT('',(8.84897443175215,-8.,-3.90512918779784E-6));
#5569=CARTESIAN_POINT('Origin',(8.84897443175212,-8.,2.99999609487078));
#5570=CARTESIAN_POINT('',(8.84897443175215,-16.,-3.90512918779784E-6));
#5571=CARTESIAN_POINT('Origin',(58.4146984106833,-8.00000000000001,2.49999609487094));
#5572=CARTESIAN_POINT('',(50.4902099491237,-8.00000000000001,1.50000181691698));
#5573=CARTESIAN_POINT('',(59.4524541799035,-8.00000000000001,1.50000181691698));
#5574=CARTESIAN_POINT('',(50.4902099491237,-8.00000000000001,-3.90512908121643E-6));
#5575=CARTESIAN_POINT('',(50.4902099491237,-8.00000000000001,1.99999895589396));
#5576=CARTESIAN_POINT('',(105.980422389614,-8.00000000000001,-3.90512892134431E-6));
#5577=CARTESIAN_POINT('',(50.4902099491237,-8.00000000000001,3.49999037282518));
#5578=CARTESIAN_POINT('',(50.4902099491237,-8.00000000000001,3.74999609487092));
#5579=CARTESIAN_POINT('',(54.4524541799035,-8.00000000000001,3.49999037282518));
#5580=CARTESIAN_POINT('',(105.980422389614,-8.00000000000001,-3.90512892134431E-6));
#5581=CARTESIAN_POINT('Origin',(50.4902099491237,-8.00000000000001,4.9999960948709));
#5582=CARTESIAN_POINT('',(50.4902099491237,-14.,3.49999037282518));
#5583=CARTESIAN_POINT('',(50.4902099491237,-14.,6.66819775988521));
#5584=CARTESIAN_POINT('',(50.4902099491237,-8.00000000000001,3.49999037282518));
#5585=CARTESIAN_POINT('Origin',(50.4902099491237,-8.00000000000001,3.49999037282518));
#5586=CARTESIAN_POINT('',(50.4902099491237,-14.,3.49999037282518));
#5587=CARTESIAN_POINT('Origin',(50.4902099491237,-8.00000000000001,1.50000181691698));
#5588=CARTESIAN_POINT('',(50.4902099491237,-14.,1.50000181691698));
#5589=CARTESIAN_POINT('',(50.4902099491237,-8.00000000000001,1.50000181691698));
#5590=CARTESIAN_POINT('',(50.4902099491237,-14.,-3.90512908121643E-6));
#5591=CARTESIAN_POINT('',(50.4902099491237,-14.,6.66819775988521));
#5592=CARTESIAN_POINT('',(50.4902099491237,-12.,-3.90512892134431E-6));
#5593=CARTESIAN_POINT('Origin',(51.4902099491237,-6.99999986588956,0.999995141196762));
#5594=CARTESIAN_POINT('',(51.4902099491237,2.38418571552046E-7,0.999999909568344));
#5595=CARTESIAN_POINT('',(51.4902099491237,2.38418571552046E-7,0.291667847800766));
#5596=CARTESIAN_POINT('',(51.4902099491237,2.38418571552046E-7,0.999999909568344));
#5597=CARTESIAN_POINT('',(51.4902099491237,-13.9999999992512,-3.905330883632E-6));
#5598=CARTESIAN_POINT('',(51.4902099491237,2.38418571552046E-7,0.291667847800766));
#5599=CARTESIAN_POINT('',(51.4902099491237,-14.,0.87499704854536));
#5600=CARTESIAN_POINT('',(51.4902099491237,-1.00000000000001,1.99999418752245));
#5601=CARTESIAN_POINT('',(51.4902099491237,-1.00000000000001,1.99999418752245));
#5602=CARTESIAN_POINT('',(51.4902099491237,2.38418571552046E-7,0.999999909568344));
#5603=CARTESIAN_POINT('Origin',(55.4902099491237,-14.,4.24999323384806));
#5604=CARTESIAN_POINT('',(51.4902099491237,-14.,4.12499514119673));
#5605=CARTESIAN_POINT('Origin',(51.4902099491237,-6.99999986588956,3.99999704854539));
#5606=CARTESIAN_POINT('',(51.4902099491237,2.38418571552046E-7,4.70832434194139));
#5607=CARTESIAN_POINT('',(51.4902099491237,2.38418571552046E-7,3.99999228017381));
#5608=CARTESIAN_POINT('',(51.4902099491237,2.38418571552046E-7,4.70832434194139));
#5609=CARTESIAN_POINT('',(51.4902099491237,-1.00000000000001,2.99999800221971));
#5610=CARTESIAN_POINT('',(51.4902099491237,2.38418571552046E-7,3.99999228017381));
#5611=CARTESIAN_POINT('',(51.4902099491237,-1.00000000000001,2.99999800221971));
#5612=CARTESIAN_POINT('',(51.4902099491237,2.38418571552046E-7,4.70832434194139));
#5613=CARTESIAN_POINT('Origin',(55.4902099491237,2.38418571552046E-7,4.70832434194139));
#5614=CARTESIAN_POINT('',(55.4902099491237,2.38418571552046E-7,3.99999228017381));
#5615=CARTESIAN_POINT('',(55.4902099491237,2.38418571552046E-7,4.70832434194139));
#5616=CARTESIAN_POINT('Origin',(55.4902099491237,2.38418571552046E-7,3.99999228017381));
#5617=CARTESIAN_POINT('',(55.4902099491237,-1.00000000000001,2.99999800221971));
#5618=CARTESIAN_POINT('Origin',(55.4902099491237,-1.00000000000001,2.99999800221971));
#5619=CARTESIAN_POINT('Origin',(55.4902099491237,-13.9999999701977,4.99999609487108));
#5620=CARTESIAN_POINT('Origin',(91.7027316808383,-16.,-53.4006783930403));
#5621=CARTESIAN_POINT('Origin',(91.7027316808383,-9.00000000000001,-53.4006783930403));
#5622=CARTESIAN_POINT('Origin',(91.7027316808383,-16.,-53.4006783930403));
#5623=CARTESIAN_POINT('Origin',(105.980422389614,-16.,-3.90512890358075E-6));
#5624=CARTESIAN_POINT('',(110.980422389614,-16.,-3.90512890358075E-6));
#5625=CARTESIAN_POINT('',(80.7353161693691,-14.,-3.90512890358075E-6));
#5626=CARTESIAN_POINT('',(80.7353161693691,-14.,-3.90512890358075E-6));
#5627=CARTESIAN_POINT('',(80.7353161693691,-14.,-3.90512890358075E-6));
#5628=CARTESIAN_POINT('Origin',(55.4902099491237,2.38418571552046E-7,0.291667847800766));
#5629=CARTESIAN_POINT('',(55.4902099491237,2.38418571552046E-7,0.291667847800766));
#5630=CARTESIAN_POINT('Origin',(55.4902099491237,2.38418571552046E-7,0.999999909568344));
#5631=CARTESIAN_POINT('',(55.4902099491237,2.38418571552046E-7,0.999999909568344));
#5632=CARTESIAN_POINT('Origin',(55.4902099491237,-1.00000000000001,1.99999418752245));
#5633=CARTESIAN_POINT('',(55.4902099491237,-1.00000000000001,1.99999418752245));
#5634=CARTESIAN_POINT('Origin',(55.4902099491237,-2.00000023841859,0.999999909568344));
#5635=CARTESIAN_POINT('Origin',(55.4902099491237,-14.,0.749998955893957));
#5636=CARTESIAN_POINT('',(50.4902099491237,-14.,1.50000181691698));
#5637=CARTESIAN_POINT('Origin',(60.4902099491237,-8.00000000000001,1.50000181691698));
#5638=CARTESIAN_POINT('Origin',(50.4902099491237,-16.,100.999999909568));
#5639=CARTESIAN_POINT('',(50.4902099491237,-8.00000000000001,102.078678577114));
#5640=CARTESIAN_POINT('',(50.4902099491237,-8.00000000000001,100.999999909568));
#5641=CARTESIAN_POINT('',(50.4902099491237,-8.00000000000001,102.249999909568));
#5642=CARTESIAN_POINT('',(50.4902099491237,-14.0786711782186,102.078678577114));
#5643=CARTESIAN_POINT('',(50.4902099491237,-16.,102.078678577114));
#5644=CARTESIAN_POINT('',(50.4902099491237,-15.,103.000001907349));
#5645=CARTESIAN_POINT('',(50.4902099491237,-15.,103.000001907349));
#5646=CARTESIAN_POINT('',(50.4902099491237,-16.,103.000001907349));
#5647=CARTESIAN_POINT('',(50.4902099491237,-17.613291571013,103.000001907349));
#5648=CARTESIAN_POINT('',(50.4902099491237,-16.,100.999999909568));
#5649=CARTESIAN_POINT('',(50.4902099491237,-16.,77.7696691222254));
#5650=CARTESIAN_POINT('',(50.4902099491237,-16.,100.999999909568));
#5651=CARTESIAN_POINT('Origin',(50.4902099491237,-16.,104.799999861885));
#5652=CARTESIAN_POINT('',(50.4902099491237,-8.00000000000001,105.999999909569));
#5653=CARTESIAN_POINT('',(50.4902099491237,-8.00000000000001,104.799999861885));
#5654=CARTESIAN_POINT('',(50.4902099491237,-8.00000000000001,104.149999885727));
#5655=CARTESIAN_POINT('',(50.4902099491237,-16.,105.999999909569));
#5656=CARTESIAN_POINT('',(50.4902099491237,-16.,105.999999909568));
#5657=CARTESIAN_POINT('',(50.4902099491237,-16.,104.000005722046));
#5658=CARTESIAN_POINT('',(50.4902099491237,-16.,78.7000003970924));
#5659=CARTESIAN_POINT('',(50.4902099491237,-15.,104.000005722046));
#5660=CARTESIAN_POINT('',(50.4902099491237,-15.,104.000005722046));
#5661=CARTESIAN_POINT('',(50.4902099491237,-14.2000010917973,104.799999861885));
#5662=CARTESIAN_POINT('',(50.4902099491237,-13.9999997615814,105.));
#5663=CARTESIAN_POINT('',(50.4902099491237,-16.,104.799999861885));
#5664=CARTESIAN_POINT('Origin',(4.99999870072585,-16.,105.999999909568));
#5665=CARTESIAN_POINT('',(4.99999750863295,-8.,105.999999909568));
#5666=CARTESIAN_POINT('',(4.99999750863295,-8.,105.999999909568));
#5667=CARTESIAN_POINT('',(4.9999981046794,-9.,105.999999909568));
#5668=CARTESIAN_POINT('',(4.99999750863295,-16.,105.999999909568));
#5669=CARTESIAN_POINT('',(4.99999870072585,-16.,105.999999909568));
#5670=CARTESIAN_POINT('',(4.99999870072585,-16.,105.999999909568));
#5671=CARTESIAN_POINT('',(-2.49136704573705E-6,-16.,105.999999909568));
#5672=CARTESIAN_POINT('Origin',(9.9999995652367,-13.2,103.499999046326));
#5673=CARTESIAN_POINT('',(8.24999986969346,-13.2,103.499999046326));
#5674=CARTESIAN_POINT('Origin',(9.9999995652367,-13.2,103.499999046326));
#5675=CARTESIAN_POINT('Origin',(9.9999995652367,-16.,103.499999046326));
#5676=CARTESIAN_POINT('',(8.24999986969346,-8.,103.499999046326));
#5677=CARTESIAN_POINT('',(8.24999986969346,-16.,103.499999046326));
#5678=CARTESIAN_POINT('Origin',(9.9999995652367,-8.,103.499999046326));
#5679=CARTESIAN_POINT('Origin',(75.2228257418789,-16.,100.999999909569));
#5680=CARTESIAN_POINT('',(9.99999750863295,-16.,100.999999909568));
#5681=CARTESIAN_POINT('',(9.99999750863295,-16.,100.999999909568));
#5682=CARTESIAN_POINT('',(9.99999750863295,-9.,100.999999909568));
#5683=CARTESIAN_POINT('',(9.99999750863295,-16.,100.999999909568));
#5684=CARTESIAN_POINT('',(-2.49136704025923E-6,-9.,100.9999995123));
#5685=CARTESIAN_POINT('',(79.9288616965592,-9.00000000000001,100.999999909568));
#5686=CARTESIAN_POINT('',(-2.49136703082233E-6,-8.,100.999999909568));
#5687=CARTESIAN_POINT('',(-2.49136703180205E-6,-16.,100.999999909568));
#5688=CARTESIAN_POINT('',(-2.49136703082233E-6,-8.,100.999999909568));
#5689=CARTESIAN_POINT('Origin',(4.99999750863296,-16.,95.9999999095684));
#5690=CARTESIAN_POINT('',(4.99999750863297,-16.,65.2452060764368));
#5691=CARTESIAN_POINT('',(4.99999750863296,-16.,95.9999999095684));
#5692=CARTESIAN_POINT('',(4.99999750863296,-16.,95.9999999095684));
#5693=CARTESIAN_POINT('',(4.99999750863297,-9.,65.2452060764368));
#5694=CARTESIAN_POINT('',(4.99999750863297,-16.,65.2452060764368));
#5695=CARTESIAN_POINT('',(4.99999750863297,-9.,95.9999999095684));
#5696=CARTESIAN_POINT('',(4.99999750863297,-9.,95.9999999095684));
#5697=CARTESIAN_POINT('',(4.99999750863296,-16.,95.9999999095684));
#5698=CARTESIAN_POINT('Origin',(9.99999750863296,-16.,95.9999999095684));
#5699=CARTESIAN_POINT('Origin',(9.99999750863296,-16.,95.9999999095684));
#5700=CARTESIAN_POINT('Origin',(9.99999750863296,-9.,95.9999999095684));
#5701=CARTESIAN_POINT('Origin',(4.99999750863296,-16.,100.999999909568));
#5702=CARTESIAN_POINT('',(-2.49136704512472E-6,-16.,100.999998717475));
#5703=CARTESIAN_POINT('Origin',(4.99999750863296,-16.,100.999999909568));
#5704=CARTESIAN_POINT('Origin',(4.99999750863297,-8.,100.999999909568));
#5705=CARTESIAN_POINT('',(-2.49136704512472E-6,-16.,100.999998717475));
#5706=CARTESIAN_POINT('Origin',(-2.49136704023105E-6,-16.,61.0401448299175));
#5707=CARTESIAN_POINT('',(-2.49136704023105E-6,-16.,61.0401448299175));
#5708=CARTESIAN_POINT('',(-2.49136703275579E-6,-16.,-3.90512892134431E-6));
#5709=CARTESIAN_POINT('',(-2.4913670393738E-6,-9.,61.0401448299175));
#5710=CARTESIAN_POINT('',(-2.49136703189854E-6,-9.,-3.90512892134431E-6));
#5711=CARTESIAN_POINT('',(-2.49136704023105E-6,-16.,61.0401448299175));
#5712=CARTESIAN_POINT('Origin',(55.4902099491237,-15.,104.000005722046));
#5713=CARTESIAN_POINT('',(60.4902099491237,-16.,104.000005722046));
#5714=CARTESIAN_POINT('',(55.4902099491237,-16.,104.000005722046));
#5715=CARTESIAN_POINT('',(60.4902099491237,-15.,104.000005722046));
#5716=CARTESIAN_POINT('',(60.4902099491237,-15.,104.000005722046));
#5717=CARTESIAN_POINT('',(55.4902099491237,-15.,104.000005722046));
#5718=CARTESIAN_POINT('Origin',(55.4902099491237,-14.2000010917973,104.799999861885));
#5719=CARTESIAN_POINT('',(60.4902099491237,-14.2000010917973,104.799999861885));
#5720=CARTESIAN_POINT('',(60.4902099491237,-13.9999997615814,105.));
#5721=CARTESIAN_POINT('',(57.9902099491237,-14.2000010917973,104.799999861885));
#5722=CARTESIAN_POINT('Origin',(55.4902099491237,-15.,103.000001907349));
#5723=CARTESIAN_POINT('',(60.4902099491237,-14.0786711782186,102.078678577114));
#5724=CARTESIAN_POINT('',(52.9902099491237,-14.0786711782186,102.078678577114));
#5725=CARTESIAN_POINT('',(60.4902099491237,-15.,103.000001907349));
#5726=CARTESIAN_POINT('',(60.4902099491237,-15.,103.000001907349));
#5727=CARTESIAN_POINT('',(55.4902099491237,-15.,103.000001907349));
#5728=CARTESIAN_POINT('Origin',(55.4902099491237,-16.,103.000001907349));
#5729=CARTESIAN_POINT('',(60.4902099491237,-16.,103.000001907349));
#5730=CARTESIAN_POINT('',(60.4902099491237,-17.613291571013,103.000001907349));
#5731=CARTESIAN_POINT('',(55.4902099491237,-16.,103.000001907349));
#5732=CARTESIAN_POINT('Origin',(55.4902099491237,-16.,52.9999980022196));
#5733=CARTESIAN_POINT('',(104.252765939044,-16.,100.878679694998));
#5734=CARTESIAN_POINT('',(20.9321760059474,-16.,17.5580486346965));
#5735=CARTESIAN_POINT('',(102.131450069058,-16.,105.999999909568));
#5736=CARTESIAN_POINT('Origin',(102.131445466495,-16.,102.999999909569));
#5737=CARTESIAN_POINT('',(60.4902099491237,-16.,105.999999909569));
#5738=CARTESIAN_POINT('',(-2.49136704573705E-6,-16.,105.999999909568));
#5739=CARTESIAN_POINT('',(60.4902099491237,-16.,78.7000003970924));
#5740=CARTESIAN_POINT('',(78.0377000859664,-16.,78.199171079613));
#5741=CARTESIAN_POINT('Origin',(19.277688217409,-16.,159.40067439748));
#5742=CARTESIAN_POINT('',(81.3189100147365,-16.,80.6776794482952));
#5743=CARTESIAN_POINT('',(77.8756307483791,-16.,78.0767497112041));
#5744=CARTESIAN_POINT('',(83.2198404193996,-16.,84.6014246036297));
#5745=CARTESIAN_POINT('Origin',(78.2198382097572,-16.,84.6014246036297));
#5746=CARTESIAN_POINT('',(83.2198404193996,-16.,91.2703653861766));
#5747=CARTESIAN_POINT('',(83.2198404193996,-16.,91.2703653861766));
#5748=CARTESIAN_POINT('',(90.0482438923,-16.,88.4419473697429));
#5749=CARTESIAN_POINT('Origin',(87.21982630964,-16.,91.2703640823622));
#5750=CARTESIAN_POINT('',(6.72763826472058,-16.,5.1213161121643));
#5751=CARTESIAN_POINT('',(60.4902099491237,-16.,100.999999909569));
#5752=CARTESIAN_POINT('',(60.4902099491237,-16.,77.5393382896666));
#5753=CARTESIAN_POINT('',(75.2228257418789,-16.,100.999999909569));
#5754=CARTESIAN_POINT('',(9.99999750863295,-16.,100.999999909568));
#5755=CARTESIAN_POINT('',(78.2228256672992,-16.,97.9993309712914));
#5756=CARTESIAN_POINT('Origin',(75.2228257418789,-16.,97.9999999095685));
#5757=CARTESIAN_POINT('',(78.2198380979424,-16.,84.601424987681));
#5758=CARTESIAN_POINT('',(78.2198382097572,-16.,84.6014246036297));
#5759=CARTESIAN_POINT('Origin',(19.277688217409,-16.,159.40067439748));
#5760=CARTESIAN_POINT('Origin',(50.4902099491237,-16.,102.078678577114));
#5761=CARTESIAN_POINT('',(60.4902099491237,-8.00000000000001,102.078678577114));
#5762=CARTESIAN_POINT('',(51.5279657183439,-8.00000000000001,102.078678577114));
#5763=CARTESIAN_POINT('',(60.4902099491237,-16.,102.078678577114));
#5764=CARTESIAN_POINT('Origin',(52.5657214875641,-8.00000000000001,103.499999909568));
#5765=CARTESIAN_POINT('',(60.4902099491237,-8.00000000000001,104.799999861885));
#5766=CARTESIAN_POINT('',(56.5279657183439,-8.00000000000001,104.799999861885));
#5767=CARTESIAN_POINT('',(60.4902099491237,-8.00000000000001,105.999999909569));
#5768=CARTESIAN_POINT('',(60.4902099491237,-8.00000000000001,104.749999909569));
#5769=CARTESIAN_POINT('',(102.131445466495,-8.00000000000001,105.999999909569));
#5770=CARTESIAN_POINT('',(4.99999750863295,-8.,105.999999909568));
#5771=CARTESIAN_POINT('',(104.367513443995,-8.00000000000001,100.999999909568));
#5772=CARTESIAN_POINT('Origin',(102.131445466495,-8.00000000000001,102.999999909569));
#5773=CARTESIAN_POINT('',(60.4902099491237,-8.00000000000001,100.999999909569));
#5774=CARTESIAN_POINT('',(-2.49136703082233E-6,-8.,100.999999909568));
#5775=CARTESIAN_POINT('',(60.4902099491237,-8.00000000000001,102.789339243341));
#5776=CARTESIAN_POINT('Origin',(104.252765939044,-16.,100.878679694998));
#5777=CARTESIAN_POINT('',(104.252765939044,-9.00000000000001,100.878679694998));
#5778=CARTESIAN_POINT('',(20.9321760059474,-9.,17.5580486346965));
#5779=CARTESIAN_POINT('',(104.252765939044,-16.,100.878679694998));
#5780=CARTESIAN_POINT('Origin',(19.277688217409,-16.,159.40067439748));
#5781=CARTESIAN_POINT('',(78.0377000859664,-9.00000000000001,78.199171079613));
#5782=CARTESIAN_POINT('Origin',(19.277688217409,-9.,159.40067439748));
#5783=CARTESIAN_POINT('',(78.0377000859664,-16.,78.199171079613));
#5784=CARTESIAN_POINT('Origin',(55.4902099491237,-9.00000000000001,52.9999980022196));
#5785=CARTESIAN_POINT('',(90.0482438923,-9.00000000000001,88.4419473697429));
#5786=CARTESIAN_POINT('',(6.72763826472058,-9.,5.1213161121643));
#5787=CARTESIAN_POINT('',(83.2198404193996,-9.00000000000001,91.2703653861766));
#5788=CARTESIAN_POINT('Origin',(87.21982630964,-9.00000000000001,91.2703640823622));
#5789=CARTESIAN_POINT('',(83.2198404193996,-9.00000000000001,84.6014246036297));
#5790=CARTESIAN_POINT('',(83.2198404193996,-9.00000000000001,91.2703653861766));
#5791=CARTESIAN_POINT('',(81.3189100147365,-9.00000000000001,80.6776794482952));
#5792=CARTESIAN_POINT('Origin',(78.2198382097572,-9.00000000000001,84.6014246036297));
#5793=CARTESIAN_POINT('',(77.8756307483791,-9.00000000000001,78.0767497112041));
#5794=CARTESIAN_POINT('',(78.2198380979424,-9.00000000000001,84.601424987681));
#5795=CARTESIAN_POINT('Origin',(19.277688217409,-9.,159.40067439748));
#5796=CARTESIAN_POINT('',(78.2228256672992,-9.00000000000001,97.9993309712914));
#5797=CARTESIAN_POINT('',(78.2198382097572,-9.00000000000001,84.6014246036297));
#5798=CARTESIAN_POINT('',(75.2228257418789,-9.00000000000001,100.999999909569));
#5799=CARTESIAN_POINT('Origin',(75.2228257418789,-9.00000000000001,97.9999999095685));
#5800=CARTESIAN_POINT('',(104.367513443995,-9.00000000000001,100.999999909568));
#5801=CARTESIAN_POINT('',(79.9288616965592,-9.00000000000001,100.999999909568));
#5802=CARTESIAN_POINT('Origin',(102.131445466495,-9.00000000000001,102.999999909569));
#5803=CARTESIAN_POINT('Origin',(60.4902099491237,-16.,102.078678577114));
#5804=CARTESIAN_POINT('',(60.4902099491237,-16.,100.999999909569));
#5805=CARTESIAN_POINT('Origin',(60.4902099491237,-16.,104.799999861885));
#5806=CARTESIAN_POINT('',(60.4902099491237,-16.,104.799999861885));
#5807=CARTESIAN_POINT('Origin',(60.4902099491237,-16.,105.999999909569));
#5808=CARTESIAN_POINT('',(60.4902099491237,-16.,105.999999909568));
#5809=CARTESIAN_POINT('Origin',(75.2228257418789,-16.,100.999999909569));
#5810=CARTESIAN_POINT('',(104.367513443995,-16.,100.999999909568));
#5811=CARTESIAN_POINT('',(75.2228257418789,-16.,100.999999909569));
#5812=CARTESIAN_POINT('Origin',(75.2228257418789,-16.,97.9999999095685));
#5813=CARTESIAN_POINT('',(78.2228256672992,-16.,97.9993309712914));
#5814=CARTESIAN_POINT('Origin',(78.2198382097572,-16.,84.6014246036297));
#5815=CARTESIAN_POINT('',(78.2198382097572,-16.,84.6014246036297));
#5816=CARTESIAN_POINT('Origin',(19.277688217409,-16.,159.40067439748));
#5817=CARTESIAN_POINT('Origin',(81.3189100147365,-16.,80.6776794482952));
#5818=CARTESIAN_POINT('',(81.3189100147365,-16.,80.6776794482952));
#5819=CARTESIAN_POINT('Origin',(78.2198382097572,-16.,84.6014246036297));
#5820=CARTESIAN_POINT('',(83.2198404193996,-16.,84.6014246036297));
#5821=CARTESIAN_POINT('Origin',(83.2198404193996,-16.,91.2703653861766));
#5822=CARTESIAN_POINT('',(83.2198404193996,-16.,91.2703653861766));
#5823=CARTESIAN_POINT('Origin',(87.21982630964,-16.,91.2703640823622));
#5824=CARTESIAN_POINT('',(90.0482438923,-16.,88.4419473697429));
#5825=CARTESIAN_POINT('Origin',(4.99999870072585,-16.,105.999999909568));
#5826=CARTESIAN_POINT('',(102.131447767777,-9.00000000000001,105.999999909569));
#5827=CARTESIAN_POINT('',(102.131450069058,-16.,105.999999909568));
#5828=CARTESIAN_POINT('',(102.131445466495,-16.,105.999999909569));
#5829=CARTESIAN_POINT('Origin',(102.131445466495,-16.,102.999999909569));
#5830=CARTESIAN_POINT('Origin',(6.72763826472058,-16.,5.1213161121643));
#5831=CARTESIAN_POINT('',(0.,0.,0.));
#5832=CARTESIAN_POINT('Origin',(10.0000045479708,-2.8,103.499999046326));
#5833=CARTESIAN_POINT('',(8.50000441279955,-2.8,103.499999046326));
#5834=CARTESIAN_POINT('Origin',(10.0000045479708,-2.8,103.499999046326));
#5835=CARTESIAN_POINT('Origin',(10.0000045479708,-8.,103.499999046326));
#5836=CARTESIAN_POINT('',(8.50000441279955,-12.,103.499999046326));
#5837=CARTESIAN_POINT('Origin',(10.0000045479708,-12.,103.499999046326));
#5838=CARTESIAN_POINT('',(8.50000441279957,-8.,103.499999046326));
#5839=CARTESIAN_POINT('Origin',(10.0000045479708,-12.,103.499999046326));
#5840=CARTESIAN_POINT('',(0.,0.,0.));
#5841=CARTESIAN_POINT('Origin',(100.979994297411,-4.00000000000001,103.500004749034));
#5842=CARTESIAN_POINT('',(102.479993922177,-12.,103.500004749034));
#5843=CARTESIAN_POINT('Origin',(100.979994297411,-12.,103.500004749034));
#5844=CARTESIAN_POINT('',(102.479993922177,-4.00000000000001,103.500004749034));
#5845=CARTESIAN_POINT('',(102.479993922178,-4.00000000000001,103.500004749034));
#5846=CARTESIAN_POINT('Origin',(100.979994297411,-4.00000000000001,103.500004749034));
#5847=CARTESIAN_POINT('Origin',(100.979994297411,-4.00000000000001,103.500004749034));
#5848=CARTESIAN_POINT('Origin',(100.979994297411,-12.,103.500004749034));
#5849=CARTESIAN_POINT('',(0.,0.,0.));
#5850=CARTESIAN_POINT('Origin',(10.0000020566038,-4.00000000000001,2.50000086324266));
#5851=CARTESIAN_POINT('',(11.500002191775,-12.,2.50000086324266));
#5852=CARTESIAN_POINT('Origin',(10.0000020566038,-12.,2.50000086324266));
#5853=CARTESIAN_POINT('',(11.500002191775,-4.00000000000001,2.50000086324266));
#5854=CARTESIAN_POINT('',(11.500002191775,-4.00000000000001,2.50000086324266));
#5855=CARTESIAN_POINT('Origin',(10.0000020566038,-4.00000000000001,2.50000086324266));
#5856=CARTESIAN_POINT('Origin',(10.0000020566038,-4.00000000000001,2.50000086324266));
#5857=CARTESIAN_POINT('Origin',(10.0000020566038,-12.,2.50000086324266));
#5858=CARTESIAN_POINT('',(0.,0.,0.));
#5859=CARTESIAN_POINT('Origin',(55.4902124404907,-12.0000001341105,105.854167938232));
#5860=CARTESIAN_POINT('',(53.4902124404907,-11.9018738839031,101.14418999359));
#5861=CARTESIAN_POINT('Origin',(55.4902124404907,-11.9018738839031,101.14418999359));
#5862=CARTESIAN_POINT('',(53.4902124404907,-12.0000001341105,105.854167938232));
#5863=CARTESIAN_POINT('',(53.4902124404907,-12.0000001341105,105.854167938232));
#5864=CARTESIAN_POINT('Origin',(55.4902124404907,-12.0000001341105,105.854167938232));
#5865=CARTESIAN_POINT('Origin',(55.4902124404907,-12.0000001341105,105.854167938232));
#5866=CARTESIAN_POINT('Origin',(55.4902124404907,-11.9018738839031,101.14418999359));
#5867=CARTESIAN_POINT('',(0.,0.,0.));
#5868=CARTESIAN_POINT('Origin',(100.979996788778,-2.8,2.49999516053467));
#5869=CARTESIAN_POINT('',(99.4799971640107,-2.8,2.49999516053467));
#5870=CARTESIAN_POINT('Origin',(100.979996788778,-2.8,2.49999516053467));
#5871=CARTESIAN_POINT('Origin',(100.979996788778,-8.,2.49999516053467));
#5872=CARTESIAN_POINT('',(99.4799971640107,-12.,2.49999516053467));
#5873=CARTESIAN_POINT('Origin',(100.979996788778,-12.,2.49999516053467));
#5874=CARTESIAN_POINT('',(99.4799971640111,-8.,2.49999516053467));
#5875=CARTESIAN_POINT('Origin',(100.979996788778,-12.,2.49999516053467));
#5876=CARTESIAN_POINT('',(0.,0.,0.));
#5877=CARTESIAN_POINT('Origin',(55.4902124404907,-4.00000013411045,0.145828066207017));
#5878=CARTESIAN_POINT('',(53.4902124404907,-4.00000013411045,0.145828066207017));
#5879=CARTESIAN_POINT('Origin',(55.4902124404907,-4.00000013411045,0.145828066207017));
#5880=CARTESIAN_POINT('',(53.4902124404907,-3.90187388390307,4.85580601084967));
#5881=CARTESIAN_POINT('',(53.4902124404907,-4.00000013411045,0.145828066207016));
#5882=CARTESIAN_POINT('Origin',(55.4902124404907,-3.90187388390307,4.85580601084967));
#5883=CARTESIAN_POINT('Origin',(55.4902124404907,-4.00000013411045,0.145828066207017));
#5884=CARTESIAN_POINT('Origin',(55.4902124404907,-3.90187388390307,4.85580601084967));
#5885=CARTESIAN_POINT('',(0.,0.,0.));
#5886=CARTESIAN_POINT('',(0.,0.,0.));
#5887=CARTESIAN_POINT('',(0.,0.,0.));
#5888=CARTESIAN_POINT('',(0.,0.,0.));
#5889=CARTESIAN_POINT('',(0.,0.,0.));
#5890=CARTESIAN_POINT('',(0.,0.,0.));
#5891=CARTESIAN_POINT('',(0.,0.,0.));
#5892=CARTESIAN_POINT('',(0.,0.,0.));
#5893=UNCERTAINTY_MEASURE_WITH_UNIT(LENGTH_MEASURE(0.01),#5913,
'DISTANCE_ACCURACY_VALUE',
'Maximum model space distance between geometric entities at asserted c
onnectivities');
#5894=UNCERTAINTY_MEASURE_WITH_UNIT(LENGTH_MEASURE(0.01),#5913,
'DISTANCE_ACCURACY_VALUE',
'Maximum model space distance between geometric entities at asserted c
onnectivities');
#5895=UNCERTAINTY_MEASURE_WITH_UNIT(LENGTH_MEASURE(0.01),#5913,
'DISTANCE_ACCURACY_VALUE',
'Maximum model space distance between geometric entities at asserted c
onnectivities');
#5896=UNCERTAINTY_MEASURE_WITH_UNIT(LENGTH_MEASURE(0.01),#5913,
'DISTANCE_ACCURACY_VALUE',
'Maximum model space distance between geometric entities at asserted c
onnectivities');
#5897=UNCERTAINTY_MEASURE_WITH_UNIT(LENGTH_MEASURE(0.01),#5913,
'DISTANCE_ACCURACY_VALUE',
'Maximum model space distance between geometric entities at asserted c
onnectivities');
#5898=UNCERTAINTY_MEASURE_WITH_UNIT(LENGTH_MEASURE(0.01),#5913,
'DISTANCE_ACCURACY_VALUE',
'Maximum model space distance between geometric entities at asserted c
onnectivities');
#5899=UNCERTAINTY_MEASURE_WITH_UNIT(LENGTH_MEASURE(0.01),#5913,
'DISTANCE_ACCURACY_VALUE',
'Maximum model space distance between geometric entities at asserted c
onnectivities');
#5900=UNCERTAINTY_MEASURE_WITH_UNIT(LENGTH_MEASURE(0.01),#5913,
'DISTANCE_ACCURACY_VALUE',
'Maximum model space distance between geometric entities at asserted c
onnectivities');
#5901=UNCERTAINTY_MEASURE_WITH_UNIT(LENGTH_MEASURE(0.01),#5913,
'DISTANCE_ACCURACY_VALUE',
'Maximum model space distance between geometric entities at asserted c
onnectivities');
#5902=UNCERTAINTY_MEASURE_WITH_UNIT(LENGTH_MEASURE(0.01),#5913,
'DISTANCE_ACCURACY_VALUE',
'Maximum model space distance between geometric entities at asserted c
onnectivities');
#5903=(
GEOMETRIC_REPRESENTATION_CONTEXT(3)
GLOBAL_UNCERTAINTY_ASSIGNED_CONTEXT((#5893))
GLOBAL_UNIT_ASSIGNED_CONTEXT((#5913,#5915,#5916))
REPRESENTATION_CONTEXT('','3D')
);
#5904=(
GEOMETRIC_REPRESENTATION_CONTEXT(3)
GLOBAL_UNCERTAINTY_ASSIGNED_CONTEXT((#5894))
GLOBAL_UNIT_ASSIGNED_CONTEXT((#5913,#5915,#5916))
REPRESENTATION_CONTEXT('','3D')
);
#5905=(
GEOMETRIC_REPRESENTATION_CONTEXT(3)
GLOBAL_UNCERTAINTY_ASSIGNED_CONTEXT((#5895))
GLOBAL_UNIT_ASSIGNED_CONTEXT((#5913,#5915,#5916))
REPRESENTATION_CONTEXT('','3D')
);
#5906=(
GEOMETRIC_REPRESENTATION_CONTEXT(3)
GLOBAL_UNCERTAINTY_ASSIGNED_CONTEXT((#5896))
GLOBAL_UNIT_ASSIGNED_CONTEXT((#5913,#5915,#5916))
REPRESENTATION_CONTEXT('','3D')
);
#5907=(
GEOMETRIC_REPRESENTATION_CONTEXT(3)
GLOBAL_UNCERTAINTY_ASSIGNED_CONTEXT((#5897))
GLOBAL_UNIT_ASSIGNED_CONTEXT((#5913,#5915,#5916))
REPRESENTATION_CONTEXT('','3D')
);
#5908=(
GEOMETRIC_REPRESENTATION_CONTEXT(3)
GLOBAL_UNCERTAINTY_ASSIGNED_CONTEXT((#5898))
GLOBAL_UNIT_ASSIGNED_CONTEXT((#5913,#5915,#5916))
REPRESENTATION_CONTEXT('','3D')
);
#5909=(
GEOMETRIC_REPRESENTATION_CONTEXT(3)
GLOBAL_UNCERTAINTY_ASSIGNED_CONTEXT((#5899))
GLOBAL_UNIT_ASSIGNED_CONTEXT((#5913,#5915,#5916))
REPRESENTATION_CONTEXT('','3D')
);
#5910=(
GEOMETRIC_REPRESENTATION_CONTEXT(3)
GLOBAL_UNCERTAINTY_ASSIGNED_CONTEXT((#5900))
GLOBAL_UNIT_ASSIGNED_CONTEXT((#5913,#5915,#5916))
REPRESENTATION_CONTEXT('','3D')
);
#5911=(
GEOMETRIC_REPRESENTATION_CONTEXT(3)
GLOBAL_UNCERTAINTY_ASSIGNED_CONTEXT((#5901))
GLOBAL_UNIT_ASSIGNED_CONTEXT((#5913,#5915,#5916))
REPRESENTATION_CONTEXT('','3D')
);
#5912=(
GEOMETRIC_REPRESENTATION_CONTEXT(3)
GLOBAL_UNCERTAINTY_ASSIGNED_CONTEXT((#5902))
GLOBAL_UNIT_ASSIGNED_CONTEXT((#5913,#5915,#5916))
REPRESENTATION_CONTEXT('','3D')
);
#5913=(
LENGTH_UNIT()
NAMED_UNIT(*)
SI_UNIT(.MILLI.,.METRE.)
);
#5914=(
LENGTH_UNIT()
NAMED_UNIT(*)
SI_UNIT($,.METRE.)
);
#5915=(
NAMED_UNIT(*)
PLANE_ANGLE_UNIT()
SI_UNIT($,.RADIAN.)
);
#5916=(
NAMED_UNIT(*)
SI_UNIT($,.STERADIAN.)
SOLID_ANGLE_UNIT()
);
#5917=SHAPE_DEFINITION_REPRESENTATION(#5926,#5943);
#5918=SHAPE_DEFINITION_REPRESENTATION(#5927,#5944);
#5919=SHAPE_DEFINITION_REPRESENTATION(#5928,#5945);
#5920=SHAPE_DEFINITION_REPRESENTATION(#5929,#5946);
#5921=SHAPE_DEFINITION_REPRESENTATION(#5930,#5947);
#5922=SHAPE_DEFINITION_REPRESENTATION(#5931,#5948);
#5923=SHAPE_DEFINITION_REPRESENTATION(#5932,#5949);
#5924=SHAPE_DEFINITION_REPRESENTATION(#5933,#5950);
#5925=SHAPE_DEFINITION_REPRESENTATION(#5934,#5951);
#5926=PRODUCT_DEFINITION_SHAPE('',$,#5953);
#5927=PRODUCT_DEFINITION_SHAPE('',$,#5954);
#5928=PRODUCT_DEFINITION_SHAPE('',$,#5955);
#5929=PRODUCT_DEFINITION_SHAPE('',$,#5956);
#5930=PRODUCT_DEFINITION_SHAPE('',$,#5957);
#5931=PRODUCT_DEFINITION_SHAPE('',$,#5958);
#5932=PRODUCT_DEFINITION_SHAPE('',$,#5959);
#5933=PRODUCT_DEFINITION_SHAPE('',$,#5960);
#5934=PRODUCT_DEFINITION_SHAPE('',$,#5961);
#5935=PRODUCT_DEFINITION_SHAPE($,$,#35);
#5936=PRODUCT_DEFINITION_SHAPE($,$,#36);
#5937=PRODUCT_DEFINITION_SHAPE($,$,#37);
#5938=PRODUCT_DEFINITION_SHAPE($,$,#38);
#5939=PRODUCT_DEFINITION_SHAPE($,$,#39);
#5940=PRODUCT_DEFINITION_SHAPE($,$,#40);
#5941=PRODUCT_DEFINITION_SHAPE($,$,#41);
#5942=PRODUCT_DEFINITION_SHAPE($,$,#42);
#5943=SHAPE_REPRESENTATION('',(#3567,#3878,#3879,#3880,#3881,#3882,#3883,
#3884,#3885),#5903);
#5944=SHAPE_REPRESENTATION('',(#3568),#5904);
#5945=SHAPE_REPRESENTATION('',(#3704),#5905);
#5946=SHAPE_REPRESENTATION('',(#3842),#5906);
#5947=SHAPE_REPRESENTATION('',(#3848),#5907);
#5948=SHAPE_REPRESENTATION('',(#3854),#5908);
#5949=SHAPE_REPRESENTATION('',(#3860),#5909);
#5950=SHAPE_REPRESENTATION('',(#3866),#5910);
#5951=SHAPE_REPRESENTATION('',(#3872),#5911);
#5952=PRODUCT_DEFINITION_CONTEXT('part definition',#5981,'design');
#5953=PRODUCT_DEFINITION('BR-159','BR-159',#5962,#5952);
#5954=PRODUCT_DEFINITION('Left_Part','Left_Part',#5963,#5952);
#5955=PRODUCT_DEFINITION('Right_Part','Right_Part',#5964,#5952);
#5956=PRODUCT_DEFINITION('Pin_01','Pin_01',#5965,#5952);
#5957=PRODUCT_DEFINITION('Pin_03','Pin_03',#5966,#5952);
#5958=PRODUCT_DEFINITION('Pin_04','Pin_04',#5967,#5952);
#5959=PRODUCT_DEFINITION('Pin_05','Pin_05',#5968,#5952);
#5960=PRODUCT_DEFINITION('Pin_02','Pin_02',#5969,#5952);
#5961=PRODUCT_DEFINITION('Pin_06','Pin_06',#5970,#5952);
#5962=PRODUCT_DEFINITION_FORMATION('',$,#5983);
#5963=PRODUCT_DEFINITION_FORMATION('',$,#5984);
#5964=PRODUCT_DEFINITION_FORMATION('',$,#5985);
#5965=PRODUCT_DEFINITION_FORMATION('',$,#5986);
#5966=PRODUCT_DEFINITION_FORMATION('',$,#5987);
#5967=PRODUCT_DEFINITION_FORMATION('',$,#5988);
#5968=PRODUCT_DEFINITION_FORMATION('',$,#5989);
#5969=PRODUCT_DEFINITION_FORMATION('',$,#5990);
#5970=PRODUCT_DEFINITION_FORMATION('',$,#5991);
#5971=PRODUCT_RELATED_PRODUCT_CATEGORY('BR-159','BR-159',(#5983));
#5972=PRODUCT_RELATED_PRODUCT_CATEGORY('Left_Part','Left_Part',(#5984));
#5973=PRODUCT_RELATED_PRODUCT_CATEGORY('Right_Part','Right_Part',(#5985));
#5974=PRODUCT_RELATED_PRODUCT_CATEGORY('Pin_01','Pin_01',(#5986));
#5975=PRODUCT_RELATED_PRODUCT_CATEGORY('Pin_03','Pin_03',(#5987));
#5976=PRODUCT_RELATED_PRODUCT_CATEGORY('Pin_04','Pin_04',(#5988));
#5977=PRODUCT_RELATED_PRODUCT_CATEGORY('Pin_05','Pin_05',(#5989));
#5978=PRODUCT_RELATED_PRODUCT_CATEGORY('Pin_02','Pin_02',(#5990));
#5979=PRODUCT_RELATED_PRODUCT_CATEGORY('Pin_06','Pin_06',(#5991));
#5980=APPLICATION_PROTOCOL_DEFINITION('international standard',
'automotive_design',2009,#5981);
#5981=APPLICATION_CONTEXT(
'Core Data for Automotive Mechanical Design Process');
#5982=PRODUCT_CONTEXT('part definition',#5981,'mechanical');
#5983=PRODUCT('BR-159','BR-159',$,(#5982));
#5984=PRODUCT('Left_Part','Left_Part',$,(#5982));
#5985=PRODUCT('Right_Part','Right_Part',$,(#5982));
#5986=PRODUCT('Pin_01','Pin_01',$,(#5982));
#5987=PRODUCT('Pin_03','Pin_03',$,(#5982));
#5988=PRODUCT('Pin_04','Pin_04',$,(#5982));
#5989=PRODUCT('Pin_05','Pin_05',$,(#5982));
#5990=PRODUCT('Pin_02','Pin_02',$,(#5982));
#5991=PRODUCT('Pin_06','Pin_06',$,(#5982));
#5992=PRESENTATION_STYLE_ASSIGNMENT((#5995));
#5993=PRESENTATION_STYLE_ASSIGNMENT((#5996));
#5994=PRESENTATION_STYLE_ASSIGNMENT((#5997));
#5995=SURFACE_STYLE_USAGE(.BOTH.,#5998);
#5996=SURFACE_STYLE_USAGE(.BOTH.,#5999);
#5997=SURFACE_STYLE_USAGE(.BOTH.,#6000);
#5998=SURFACE_SIDE_STYLE('',(#6001));
#5999=SURFACE_SIDE_STYLE('',(#6002));
#6000=SURFACE_SIDE_STYLE('',(#6003));
#6001=SURFACE_STYLE_FILL_AREA(#6004);
#6002=SURFACE_STYLE_FILL_AREA(#6005);
#6003=SURFACE_STYLE_FILL_AREA(#6006);
#6004=FILL_AREA_STYLE('Steel - Satin',(#6007));
#6005=FILL_AREA_STYLE('Opaque(179,179,179)',(#6008));
#6006=FILL_AREA_STYLE('Opaque(160,160,160)',(#6009));
#6007=FILL_AREA_STYLE_COLOUR('Steel - Satin',#6010);
#6008=FILL_AREA_STYLE_COLOUR('Opaque(179,179,179)',#6011);
#6009=FILL_AREA_STYLE_COLOUR('Opaque(160,160,160)',#6012);
#6010=COLOUR_RGB('Steel - Satin', 0.09019608, 0.27058824, 0.51372549);
#6011=COLOUR_RGB('Opaque(179,179,179)', 0.09019608, 0.27058824, 0.51372549);
#6012=COLOUR_RGB('Opaque(160,160,160)', 0.31764706, 0.68627451, 0.89019608);
ENDSEC;
END-ISO-10303-21;
